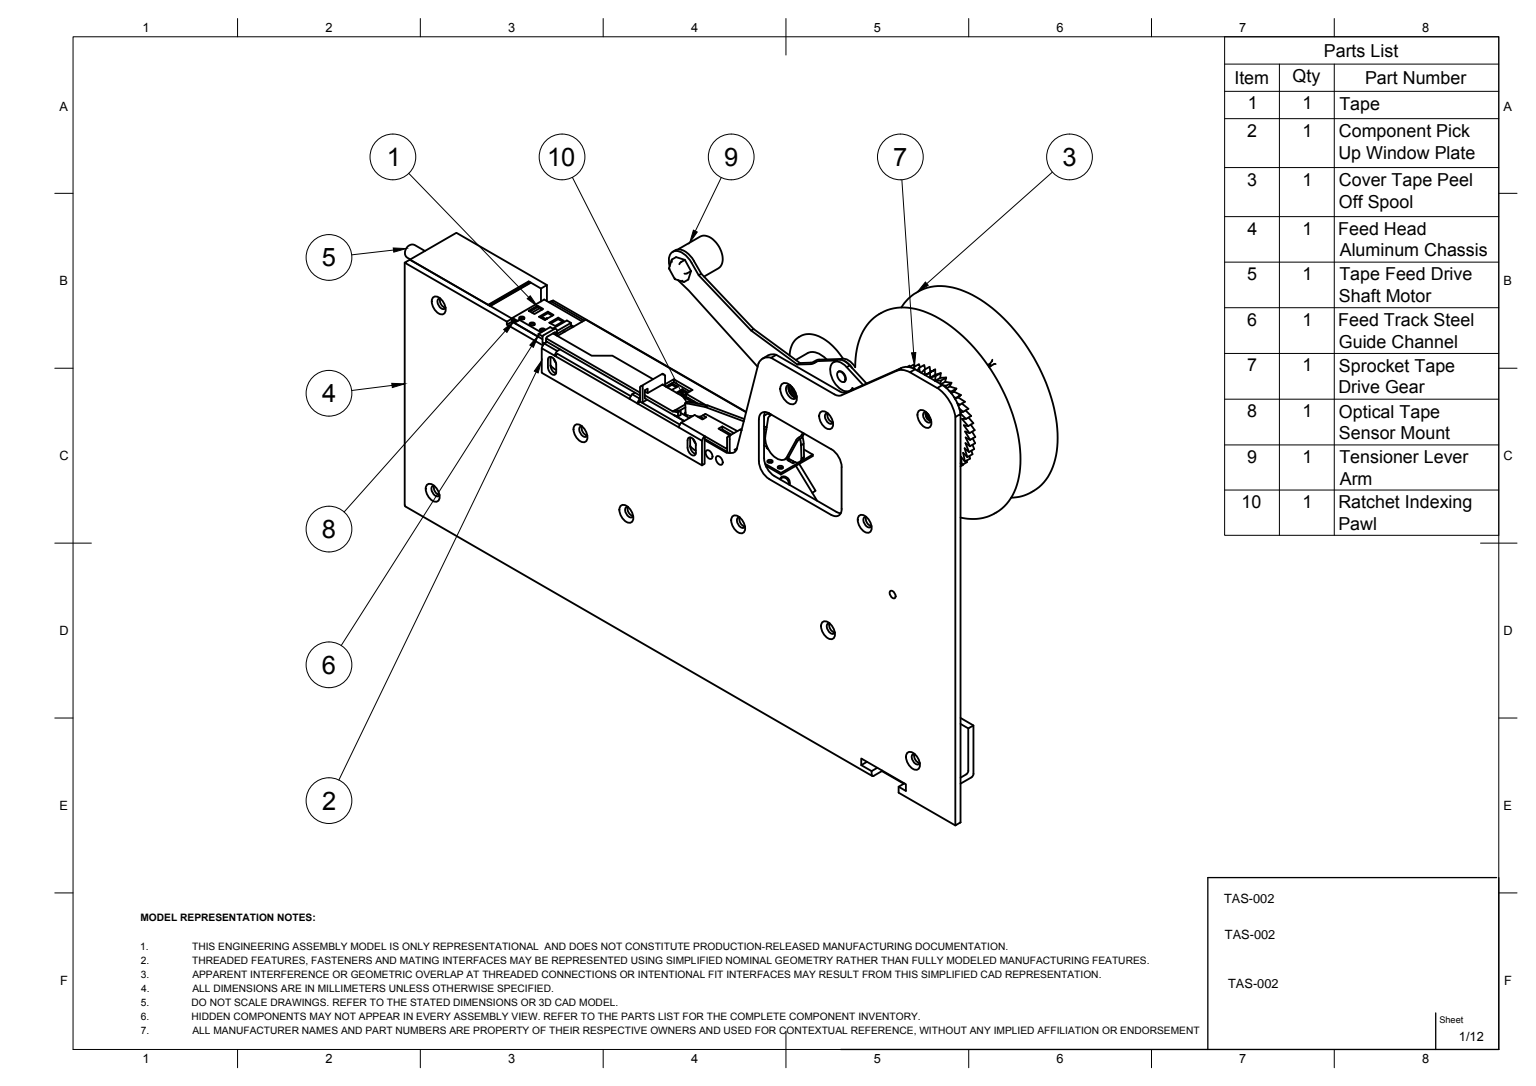
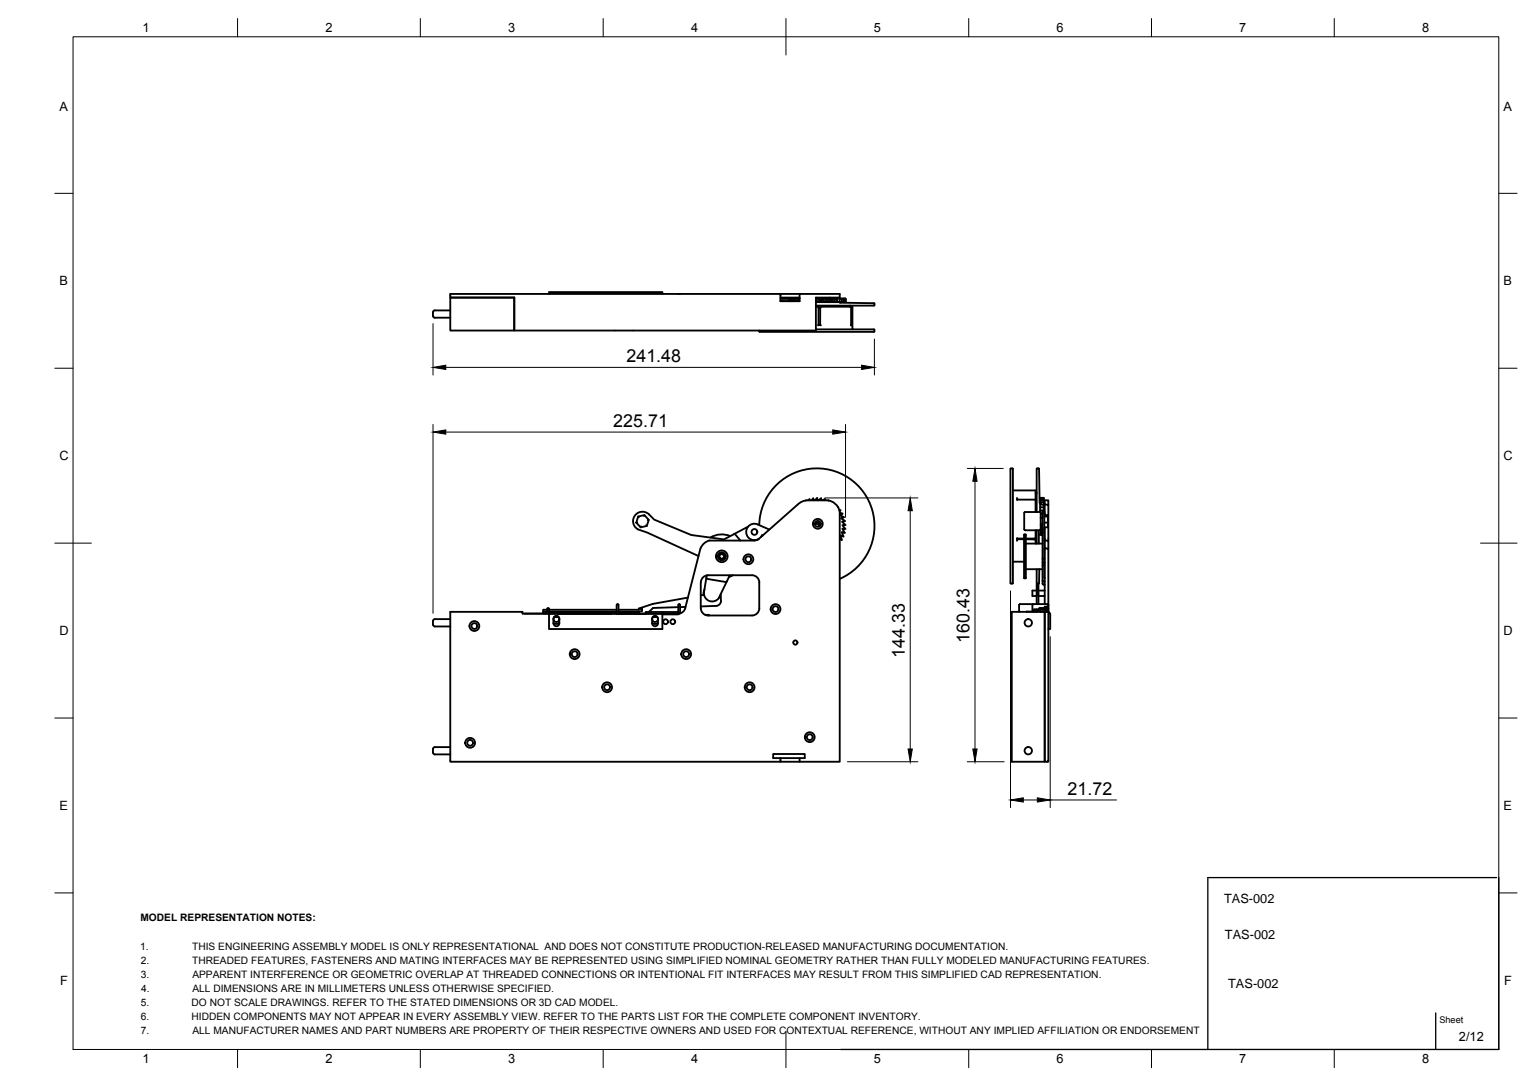
ISO-10303-21;
HEADER;
/* Generated by software containing ST-Developer
 * from STEP Tools, Inc. (www.steptools.com) 
 */

FILE_DESCRIPTION(
/* description */ ('STEP AP214'),
/* implementation_level */ '2;1');

FILE_NAME(
/* name */ 'TAS-002',
/* time_stamp */ '2026-11-04T19:38:14-08:00',
/* author */ (''),
/* organization */ (''),
/* preprocessor_version */ 'ST-DEVELOPER v20.2',
/* originating_system */ 'Autodesk Translation Framework v15.17.0.0',
/* authorisation */ '');

FILE_SCHEMA (('AUTOMOTIVE_DESIGN { 1 0 10303 214 3 1 1 }'));
ENDSEC;

DATA;
#10=MECHANICAL_DESIGN_GEOMETRIC_PRESENTATION_REPRESENTATION('',(#470,#471,
#472,#473,#474,#475,#476,#477,#478,#479),#36668);
#11=ITEM_DEFINED_TRANSFORMATION($,$,#17916,#19428);
#12=ITEM_DEFINED_TRANSFORMATION($,$,#18105,#19429);
#13=ITEM_DEFINED_TRANSFORMATION($,$,#18270,#19430);
#14=ITEM_DEFINED_TRANSFORMATION($,$,#18564,#19431);
#15=ITEM_DEFINED_TRANSFORMATION($,$,#18726,#19432);
#16=ITEM_DEFINED_TRANSFORMATION($,$,#18755,#19433);
#17=ITEM_DEFINED_TRANSFORMATION($,$,#18787,#19434);
#18=ITEM_DEFINED_TRANSFORMATION($,$,#19085,#19435);
#19=ITEM_DEFINED_TRANSFORMATION($,$,#19168,#19436);
#20=ITEM_DEFINED_TRANSFORMATION($,$,#19405,#19437);
#21=(
REPRESENTATION_RELATIONSHIP($,$,#36706,#36705)
REPRESENTATION_RELATIONSHIP_WITH_TRANSFORMATION(#11)
SHAPE_REPRESENTATION_RELATIONSHIP()
);
#22=(
REPRESENTATION_RELATIONSHIP($,$,#36707,#36705)
REPRESENTATION_RELATIONSHIP_WITH_TRANSFORMATION(#12)
SHAPE_REPRESENTATION_RELATIONSHIP()
);
#23=(
REPRESENTATION_RELATIONSHIP($,$,#36708,#36705)
REPRESENTATION_RELATIONSHIP_WITH_TRANSFORMATION(#13)
SHAPE_REPRESENTATION_RELATIONSHIP()
);
#24=(
REPRESENTATION_RELATIONSHIP($,$,#36709,#36705)
REPRESENTATION_RELATIONSHIP_WITH_TRANSFORMATION(#14)
SHAPE_REPRESENTATION_RELATIONSHIP()
);
#25=(
REPRESENTATION_RELATIONSHIP($,$,#36710,#36705)
REPRESENTATION_RELATIONSHIP_WITH_TRANSFORMATION(#15)
SHAPE_REPRESENTATION_RELATIONSHIP()
);
#26=(
REPRESENTATION_RELATIONSHIP($,$,#36711,#36705)
REPRESENTATION_RELATIONSHIP_WITH_TRANSFORMATION(#16)
SHAPE_REPRESENTATION_RELATIONSHIP()
);
#27=(
REPRESENTATION_RELATIONSHIP($,$,#36712,#36705)
REPRESENTATION_RELATIONSHIP_WITH_TRANSFORMATION(#17)
SHAPE_REPRESENTATION_RELATIONSHIP()
);
#28=(
REPRESENTATION_RELATIONSHIP($,$,#36713,#36705)
REPRESENTATION_RELATIONSHIP_WITH_TRANSFORMATION(#18)
SHAPE_REPRESENTATION_RELATIONSHIP()
);
#29=(
REPRESENTATION_RELATIONSHIP($,$,#36714,#36705)
REPRESENTATION_RELATIONSHIP_WITH_TRANSFORMATION(#19)
SHAPE_REPRESENTATION_RELATIONSHIP()
);
#30=(
REPRESENTATION_RELATIONSHIP($,$,#36715,#36705)
REPRESENTATION_RELATIONSHIP_WITH_TRANSFORMATION(#20)
SHAPE_REPRESENTATION_RELATIONSHIP()
);
#31=CONTEXT_DEPENDENT_SHAPE_REPRESENTATION(#21,#36695);
#32=CONTEXT_DEPENDENT_SHAPE_REPRESENTATION(#22,#36696);
#33=CONTEXT_DEPENDENT_SHAPE_REPRESENTATION(#23,#36697);
#34=CONTEXT_DEPENDENT_SHAPE_REPRESENTATION(#24,#36698);
#35=CONTEXT_DEPENDENT_SHAPE_REPRESENTATION(#25,#36699);
#36=CONTEXT_DEPENDENT_SHAPE_REPRESENTATION(#26,#36700);
#37=CONTEXT_DEPENDENT_SHAPE_REPRESENTATION(#27,#36701);
#38=CONTEXT_DEPENDENT_SHAPE_REPRESENTATION(#28,#36702);
#39=CONTEXT_DEPENDENT_SHAPE_REPRESENTATION(#29,#36703);
#40=CONTEXT_DEPENDENT_SHAPE_REPRESENTATION(#30,#36704);
#41=NEXT_ASSEMBLY_USAGE_OCCURRENCE('Tape:1','Tape:1','Tape:1',#36717,#36718,
'Tape:1');
#42=NEXT_ASSEMBLY_USAGE_OCCURRENCE('Component Pick Up Window Plate:1',
'Component Pick Up Window Plate:1','Component Pick Up Window Plate:1',#36717,
#36719,'Component Pick Up Window Plate:1');
#43=NEXT_ASSEMBLY_USAGE_OCCURRENCE('Cover Tape Peel Off Spool:1',
'Cover Tape Peel Off Spool:1','Cover Tape Peel Off Spool:1',#36717,#36720,
'Cover Tape Peel Off Spool:1');
#44=NEXT_ASSEMBLY_USAGE_OCCURRENCE('Feed Head Aluminum Chassis:1',
'Feed Head Aluminum Chassis:1','Feed Head Aluminum Chassis:1',#36717,#36721,
'Feed Head Aluminum Chassis:1');
#45=NEXT_ASSEMBLY_USAGE_OCCURRENCE('Tape Feed Drive Shaft Motor:1',
'Tape Feed Drive Shaft Motor:1','Tape Feed Drive Shaft Motor:1',#36717,
#36722,'Tape Feed Drive Shaft Motor:1');
#46=NEXT_ASSEMBLY_USAGE_OCCURRENCE('Feed Track Steel Guide Channel:1',
'Feed Track Steel Guide Channel:1','Feed Track Steel Guide Channel:1',#36717,
#36723,'Feed Track Steel Guide Channel:1');
#47=NEXT_ASSEMBLY_USAGE_OCCURRENCE('Sprocket Tape Drive Gear:1',
'Sprocket Tape Drive Gear:1','Sprocket Tape Drive Gear:1',#36717,#36724,
'Sprocket Tape Drive Gear:1');
#48=NEXT_ASSEMBLY_USAGE_OCCURRENCE('Optical Tape Sensor Mount:1',
'Optical Tape Sensor Mount:1','Optical Tape Sensor Mount:1',#36717,#36725,
'Optical Tape Sensor Mount:1');
#49=NEXT_ASSEMBLY_USAGE_OCCURRENCE('Tensioner Lever Arm:1',
'Tensioner Lever Arm:1','Tensioner Lever Arm:1',#36717,#36726,
'Tensioner Lever Arm:1');
#50=NEXT_ASSEMBLY_USAGE_OCCURRENCE('Ratchet Indexing Pawl:1',
'Ratchet Indexing Pawl:1','Ratchet Indexing Pawl:1',#36717,#36727,
'Ratchet Indexing Pawl:1');
#51=ORIENTED_CLOSED_SHELL('',*,#17801,.F.);
#52=BREP_WITH_VOIDS('Body1',#17802,(#51));
#53=B_SPLINE_SURFACE_WITH_KNOTS('',3,1,((#33152,#33153),(#33154,#33155),
(#33156,#33157),(#33158,#33159),(#33160,#33161),(#33162,#33163),(#33164,
#33165),(#33166,#33167),(#33168,#33169),(#33170,#33171),(#33172,#33173),
(#33174,#33175),(#33176,#33177),(#33178,#33179),(#33180,#33181),(#33182,
#33183),(#33184,#33185),(#33186,#33187),(#33188,#33189)),.UNSPECIFIED.,
 .F.,.F.,.F.,(4,1,1,1,1,1,1,1,1,1,1,1,1,1,1,1,4),(2,2),(0.,0.0619654006870562,
0.122121905638296,0.180988496849837,0.239933216451894,0.299905831106524,
0.359988847476984,0.421775741741642,0.486575826421121,0.551534804619736,
0.615017542759975,0.677258616661654,0.739729962362713,0.803050102662949,
0.866495132015699,0.931973474177149,1.),(0.,0.0239999999999995),
 .UNSPECIFIED.);
#54=B_SPLINE_SURFACE_WITH_KNOTS('',3,1,((#33213,#33214),(#33215,#33216),
(#33217,#33218),(#33219,#33220),(#33221,#33222),(#33223,#33224),(#33225,
#33226),(#33227,#33228),(#33229,#33230),(#33231,#33232),(#33233,#33234),
(#33235,#33236),(#33237,#33238),(#33239,#33240),(#33241,#33242)),
 .UNSPECIFIED.,.F.,.F.,.F.,(4,1,1,1,1,1,1,1,1,1,1,1,4),(2,2),(0.,0.110802643801324,
0.212829202347773,0.306101309823115,0.390647321116006,0.46692446936085,
0.534481039284033,0.593586940965671,0.644557004508714,0.736200452629367,
0.825024025618864,0.911985584829753,1.),(0.,0.0239999999999995),
 .UNSPECIFIED.);
#55=B_SPLINE_SURFACE_WITH_KNOTS('',3,1,((#33280,#33281),(#33282,#33283),
(#33284,#33285),(#33286,#33287),(#33288,#33289),(#33290,#33291),(#33292,
#33293),(#33294,#33295),(#33296,#33297),(#33298,#33299),(#33300,#33301),
(#33302,#33303),(#33304,#33305),(#33306,#33307),(#33308,#33309)),
 .UNSPECIFIED.,.F.,.F.,.F.,(4,1,1,1,1,1,1,1,1,1,1,1,4),(2,2),(0.,0.0987013748863702,
0.195670680385855,0.292419992908961,0.391339286967469,0.444458741764931,
0.504224579154748,0.570347591406357,0.642913825979479,0.722289816523959,
0.807922721202247,0.900470366297794,1.),(0.,0.0239999999999995),
 .UNSPECIFIED.);
#56=B_SPLINE_SURFACE_WITH_KNOTS('',3,1,((#33327,#33328),(#33329,#33330),
(#33331,#33332),(#33333,#33334),(#33335,#33336),(#33337,#33338),(#33339,
#33340),(#33341,#33342),(#33343,#33344),(#33345,#33346),(#33347,#33348),
(#33349,#33350),(#33351,#33352),(#33353,#33354),(#33355,#33356),(#33357,
#33358),(#33359,#33360),(#33361,#33362),(#33363,#33364)),.UNSPECIFIED.,
 .F.,.F.,.F.,(4,1,1,1,1,1,1,1,1,1,1,1,1,1,1,1,4),(2,2),(0.,0.0694796363669832,
0.136525003539142,0.200800892873422,0.263983206913328,0.325711144761188,
0.38727051407573,0.449492780531563,0.51295519576285,0.576266397070109,0.637574966831173,
0.697901098424494,0.757558279411561,0.81658750436506,0.876645756608308,
0.937285872938128,1.),(0.,0.0240000000000054),.UNSPECIFIED.);
#57=B_SPLINE_SURFACE_WITH_KNOTS('',3,1,((#33386,#33387),(#33388,#33389),
(#33390,#33391),(#33392,#33393),(#33394,#33395),(#33396,#33397),(#33398,
#33399),(#33400,#33401),(#33402,#33403),(#33404,#33405),(#33406,#33407),
(#33408,#33409),(#33410,#33411),(#33412,#33413),(#33414,#33415),(#33416,
#33417),(#33418,#33419),(#33420,#33421),(#33422,#33423)),.UNSPECIFIED.,
 .F.,.F.,.F.,(4,1,1,1,1,1,1,1,1,1,1,1,1,1,1,1,4),(2,2),(0.,0.0687907943906199,
0.135103289431132,0.198978674310652,0.261904299780862,0.323494969367974,
0.385195377966055,0.446969238740777,0.509764776703136,0.572250568847369,
0.633405175661155,0.693251162921754,0.752583162785671,0.812579266153423,
0.873275084920192,0.93554994289503,1.),(0.,0.0239999999999995),
 .UNSPECIFIED.);
#58=B_SPLINE_SURFACE_WITH_KNOTS('',3,1,((#33449,#33450),(#33451,#33452),
(#33453,#33454),(#33455,#33456),(#33457,#33458),(#33459,#33460),(#33461,
#33462),(#33463,#33464),(#33465,#33466),(#33467,#33468),(#33469,#33470),
(#33471,#33472),(#33473,#33474),(#33475,#33476),(#33477,#33478),(#33479,
#33480),(#33481,#33482),(#33483,#33484),(#33485,#33486)),.UNSPECIFIED.,
 .F.,.F.,.F.,(4,1,1,1,1,1,1,1,1,1,1,1,1,1,1,1,4),(2,2),(0.,0.064429890715421,
0.126529667073554,0.186743666835525,0.245897683478137,0.304053106820992,
0.362195516217047,0.420654638852463,0.480330856318868,0.540662876085596,
0.600743511343268,0.661981856833518,0.724480055372708,0.789067141037209,
0.856333336778513,0.926362064011592,1.),(0.,0.0239999999999995),
 .UNSPECIFIED.);
#59=(
BOUNDED_CURVE()
B_SPLINE_CURVE(2,(#28963,#28964,#28965,#28966,#28967,#28968,#28969),
 .UNSPECIFIED.,.F.,.F.)
B_SPLINE_CURVE_WITH_KNOTS((3,2,2,3),(0.975,0.983333333333333,0.991666666666667,
1.),.UNSPECIFIED.)
CURVE()
GEOMETRIC_REPRESENTATION_ITEM()
RATIONAL_B_SPLINE_CURVE((1.,0.866025403784439,1.,0.866025403784439,1.,0.866025403784439,
1.))
REPRESENTATION_ITEM('')
);
#60=(
BOUNDED_CURVE()
B_SPLINE_CURVE(2,(#28975,#28976,#28977,#28978,#28979,#28980,#28981),
 .UNSPECIFIED.,.F.,.F.)
B_SPLINE_CURVE_WITH_KNOTS((3,2,2,3),(0.975,0.983333333333333,0.991666666666667,
1.),.UNSPECIFIED.)
CURVE()
GEOMETRIC_REPRESENTATION_ITEM()
RATIONAL_B_SPLINE_CURVE((1.,0.866025403784439,1.,0.866025403784439,1.,0.866025403784439,
1.))
REPRESENTATION_ITEM('')
);
#61=(
BOUNDED_CURVE()
B_SPLINE_CURVE(2,(#28984,#28985,#28986,#28987,#28988,#28989,#28990),
 .UNSPECIFIED.,.F.,.F.)
B_SPLINE_CURVE_WITH_KNOTS((3,2,2,3),(0.975,0.983333333333333,0.991666666666667,
1.),.UNSPECIFIED.)
CURVE()
GEOMETRIC_REPRESENTATION_ITEM()
RATIONAL_B_SPLINE_CURVE((1.,0.866025403784439,1.,0.866025403784439,1.,0.866025403784439,
1.))
REPRESENTATION_ITEM('')
);
#62=(
BOUNDED_CURVE()
B_SPLINE_CURVE(2,(#28995,#28996,#28997,#28998,#28999,#29000,#29001,#29002,
#29003,#29004,#29005,#29006,#29007),.UNSPECIFIED.,.F.,.F.)
B_SPLINE_CURVE_WITH_KNOTS((3,2,2,2,2,2,3),(0.925,0.933333333333333,0.941666666666667,
0.95,0.958333333333333,0.966666666666667,0.975),.UNSPECIFIED.)
CURVE()
GEOMETRIC_REPRESENTATION_ITEM()
RATIONAL_B_SPLINE_CURVE((1.,0.866025403784439,1.,0.866025403784439,1.,0.866025403784439,
1.,0.866025403784439,1.,0.866025403784439,1.,0.866025403784439,1.))
REPRESENTATION_ITEM('')
);
#63=(
BOUNDED_CURVE()
B_SPLINE_CURVE(2,(#29008,#29009,#29010,#29011,#29012,#29013,#29014,#29015,
#29016,#29017,#29018,#29019,#29020),.UNSPECIFIED.,.F.,.F.)
B_SPLINE_CURVE_WITH_KNOTS((3,2,2,2,2,2,3),(0.925,0.933333333333333,0.941666666666667,
0.95,0.958333333333333,0.966666666666667,0.975),.UNSPECIFIED.)
CURVE()
GEOMETRIC_REPRESENTATION_ITEM()
RATIONAL_B_SPLINE_CURVE((1.,0.866025403784439,1.,0.866025403784439,1.,0.866025403784439,
1.,0.866025403784439,1.,0.866025403784439,1.,0.866025403784439,1.))
REPRESENTATION_ITEM('')
);
#64=(
BOUNDED_CURVE()
B_SPLINE_CURVE(2,(#29025,#29026,#29027,#29028,#29029,#29030,#29031,#29032,
#29033,#29034,#29035,#29036,#29037),.UNSPECIFIED.,.F.,.F.)
B_SPLINE_CURVE_WITH_KNOTS((3,2,2,2,2,2,3),(0.875,0.883333333333333,0.891666666666667,
0.9,0.908333333333333,0.916666666666667,0.925),.UNSPECIFIED.)
CURVE()
GEOMETRIC_REPRESENTATION_ITEM()
RATIONAL_B_SPLINE_CURVE((1.,0.866025403784439,1.,0.866025403784439,1.,0.866025403784439,
1.,0.866025403784439,1.,0.866025403784439,1.,0.866025403784439,1.))
REPRESENTATION_ITEM('')
);
#65=(
BOUNDED_CURVE()
B_SPLINE_CURVE(2,(#29038,#29039,#29040,#29041,#29042,#29043,#29044,#29045,
#29046,#29047,#29048,#29049,#29050),.UNSPECIFIED.,.F.,.F.)
B_SPLINE_CURVE_WITH_KNOTS((3,2,2,2,2,2,3),(0.875,0.883333333333333,0.891666666666667,
0.9,0.908333333333333,0.916666666666667,0.925),.UNSPECIFIED.)
CURVE()
GEOMETRIC_REPRESENTATION_ITEM()
RATIONAL_B_SPLINE_CURVE((1.,0.866025403784439,1.,0.866025403784439,1.,0.866025403784439,
1.,0.866025403784439,1.,0.866025403784439,1.,0.866025403784439,1.))
REPRESENTATION_ITEM('')
);
#66=(
BOUNDED_CURVE()
B_SPLINE_CURVE(2,(#29055,#29056,#29057,#29058,#29059,#29060,#29061,#29062,
#29063,#29064,#29065,#29066,#29067),.UNSPECIFIED.,.F.,.F.)
B_SPLINE_CURVE_WITH_KNOTS((3,2,2,2,2,2,3),(0.825,0.833333333333333,0.841666666666667,
0.85,0.858333333333333,0.866666666666667,0.875),.UNSPECIFIED.)
CURVE()
GEOMETRIC_REPRESENTATION_ITEM()
RATIONAL_B_SPLINE_CURVE((1.,0.866025403784439,1.,0.866025403784439,1.,0.866025403784439,
1.,0.866025403784439,1.,0.866025403784439,1.,0.866025403784439,1.))
REPRESENTATION_ITEM('')
);
#67=(
BOUNDED_CURVE()
B_SPLINE_CURVE(2,(#29068,#29069,#29070,#29071,#29072,#29073,#29074,#29075,
#29076,#29077,#29078,#29079,#29080),.UNSPECIFIED.,.F.,.F.)
B_SPLINE_CURVE_WITH_KNOTS((3,2,2,2,2,2,3),(0.825,0.833333333333333,0.841666666666667,
0.85,0.858333333333333,0.866666666666667,0.875),.UNSPECIFIED.)
CURVE()
GEOMETRIC_REPRESENTATION_ITEM()
RATIONAL_B_SPLINE_CURVE((1.,0.866025403784439,1.,0.866025403784439,1.,0.866025403784439,
1.,0.866025403784439,1.,0.866025403784439,1.,0.866025403784439,1.))
REPRESENTATION_ITEM('')
);
#68=(
BOUNDED_CURVE()
B_SPLINE_CURVE(2,(#29085,#29086,#29087,#29088,#29089,#29090,#29091,#29092,
#29093,#29094,#29095,#29096,#29097),.UNSPECIFIED.,.F.,.F.)
B_SPLINE_CURVE_WITH_KNOTS((3,2,2,2,2,2,3),(0.775,0.783333333333333,0.791666666666667,
0.8,0.808333333333333,0.816666666666667,0.825),.UNSPECIFIED.)
CURVE()
GEOMETRIC_REPRESENTATION_ITEM()
RATIONAL_B_SPLINE_CURVE((1.,0.866025403784439,1.,0.866025403784439,1.,0.866025403784439,
1.,0.866025403784439,1.,0.866025403784439,1.,0.866025403784439,1.))
REPRESENTATION_ITEM('')
);
#69=(
BOUNDED_CURVE()
B_SPLINE_CURVE(2,(#29098,#29099,#29100,#29101,#29102,#29103,#29104,#29105,
#29106,#29107,#29108,#29109,#29110),.UNSPECIFIED.,.F.,.F.)
B_SPLINE_CURVE_WITH_KNOTS((3,2,2,2,2,2,3),(0.775,0.783333333333333,0.791666666666667,
0.8,0.808333333333333,0.816666666666667,0.825),.UNSPECIFIED.)
CURVE()
GEOMETRIC_REPRESENTATION_ITEM()
RATIONAL_B_SPLINE_CURVE((1.,0.866025403784439,1.,0.866025403784439,1.,0.866025403784439,
1.,0.866025403784439,1.,0.866025403784439,1.,0.866025403784439,1.))
REPRESENTATION_ITEM('')
);
#70=(
BOUNDED_CURVE()
B_SPLINE_CURVE(2,(#29115,#29116,#29117,#29118,#29119,#29120,#29121,#29122,
#29123,#29124,#29125,#29126,#29127),.UNSPECIFIED.,.F.,.F.)
B_SPLINE_CURVE_WITH_KNOTS((3,2,2,2,2,2,3),(0.725,0.733333333333333,0.741666666666667,
0.75,0.758333333333333,0.766666666666667,0.775),.UNSPECIFIED.)
CURVE()
GEOMETRIC_REPRESENTATION_ITEM()
RATIONAL_B_SPLINE_CURVE((1.,0.866025403784439,1.,0.866025403784439,1.,0.866025403784439,
1.,0.866025403784439,1.,0.866025403784439,1.,0.866025403784439,1.))
REPRESENTATION_ITEM('')
);
#71=(
BOUNDED_CURVE()
B_SPLINE_CURVE(2,(#29128,#29129,#29130,#29131,#29132,#29133,#29134,#29135,
#29136,#29137,#29138,#29139,#29140),.UNSPECIFIED.,.F.,.F.)
B_SPLINE_CURVE_WITH_KNOTS((3,2,2,2,2,2,3),(0.725,0.733333333333333,0.741666666666667,
0.75,0.758333333333333,0.766666666666667,0.775),.UNSPECIFIED.)
CURVE()
GEOMETRIC_REPRESENTATION_ITEM()
RATIONAL_B_SPLINE_CURVE((1.,0.866025403784439,1.,0.866025403784439,1.,0.866025403784439,
1.,0.866025403784439,1.,0.866025403784439,1.,0.866025403784439,1.))
REPRESENTATION_ITEM('')
);
#72=(
BOUNDED_CURVE()
B_SPLINE_CURVE(2,(#29145,#29146,#29147,#29148,#29149,#29150,#29151,#29152,
#29153,#29154,#29155,#29156,#29157),.UNSPECIFIED.,.F.,.F.)
B_SPLINE_CURVE_WITH_KNOTS((3,2,2,2,2,2,3),(0.675,0.683333333333333,0.691666666666667,
0.7,0.708333333333333,0.716666666666667,0.725),.UNSPECIFIED.)
CURVE()
GEOMETRIC_REPRESENTATION_ITEM()
RATIONAL_B_SPLINE_CURVE((1.,0.866025403784439,1.,0.866025403784439,1.,0.866025403784439,
1.,0.866025403784439,1.,0.866025403784439,1.,0.866025403784439,1.))
REPRESENTATION_ITEM('')
);
#73=(
BOUNDED_CURVE()
B_SPLINE_CURVE(2,(#29158,#29159,#29160,#29161,#29162,#29163,#29164,#29165,
#29166,#29167,#29168,#29169,#29170),.UNSPECIFIED.,.F.,.F.)
B_SPLINE_CURVE_WITH_KNOTS((3,2,2,2,2,2,3),(0.675,0.683333333333333,0.691666666666667,
0.7,0.708333333333333,0.716666666666667,0.725),.UNSPECIFIED.)
CURVE()
GEOMETRIC_REPRESENTATION_ITEM()
RATIONAL_B_SPLINE_CURVE((1.,0.866025403784439,1.,0.866025403784439,1.,0.866025403784439,
1.,0.866025403784439,1.,0.866025403784439,1.,0.866025403784439,1.))
REPRESENTATION_ITEM('')
);
#74=(
BOUNDED_CURVE()
B_SPLINE_CURVE(2,(#29175,#29176,#29177,#29178,#29179,#29180,#29181,#29182,
#29183,#29184,#29185,#29186,#29187),.UNSPECIFIED.,.F.,.F.)
B_SPLINE_CURVE_WITH_KNOTS((3,2,2,2,2,2,3),(0.625,0.633333333333333,0.641666666666667,
0.65,0.658333333333333,0.666666666666667,0.675),.UNSPECIFIED.)
CURVE()
GEOMETRIC_REPRESENTATION_ITEM()
RATIONAL_B_SPLINE_CURVE((1.,0.866025403784439,1.,0.866025403784439,1.,0.866025403784439,
1.,0.866025403784439,1.,0.866025403784439,1.,0.866025403784439,1.))
REPRESENTATION_ITEM('')
);
#75=(
BOUNDED_CURVE()
B_SPLINE_CURVE(2,(#29188,#29189,#29190,#29191,#29192,#29193,#29194,#29195,
#29196,#29197,#29198,#29199,#29200),.UNSPECIFIED.,.F.,.F.)
B_SPLINE_CURVE_WITH_KNOTS((3,2,2,2,2,2,3),(0.625,0.633333333333333,0.641666666666667,
0.65,0.658333333333333,0.666666666666667,0.675),.UNSPECIFIED.)
CURVE()
GEOMETRIC_REPRESENTATION_ITEM()
RATIONAL_B_SPLINE_CURVE((1.,0.866025403784439,1.,0.866025403784439,1.,0.866025403784439,
1.,0.866025403784439,1.,0.866025403784439,1.,0.866025403784439,1.))
REPRESENTATION_ITEM('')
);
#76=(
BOUNDED_CURVE()
B_SPLINE_CURVE(2,(#29205,#29206,#29207,#29208,#29209,#29210,#29211,#29212,
#29213,#29214,#29215,#29216,#29217),.UNSPECIFIED.,.F.,.F.)
B_SPLINE_CURVE_WITH_KNOTS((3,2,2,2,2,2,3),(0.575,0.583333333333333,0.591666666666667,
0.6,0.608333333333333,0.616666666666667,0.625),.UNSPECIFIED.)
CURVE()
GEOMETRIC_REPRESENTATION_ITEM()
RATIONAL_B_SPLINE_CURVE((1.,0.866025403784439,1.,0.866025403784439,1.,0.866025403784439,
1.,0.866025403784439,1.,0.866025403784439,1.,0.866025403784439,1.))
REPRESENTATION_ITEM('')
);
#77=(
BOUNDED_CURVE()
B_SPLINE_CURVE(2,(#29218,#29219,#29220,#29221,#29222,#29223,#29224,#29225,
#29226,#29227,#29228,#29229,#29230),.UNSPECIFIED.,.F.,.F.)
B_SPLINE_CURVE_WITH_KNOTS((3,2,2,2,2,2,3),(0.575,0.583333333333333,0.591666666666667,
0.6,0.608333333333333,0.616666666666667,0.625),.UNSPECIFIED.)
CURVE()
GEOMETRIC_REPRESENTATION_ITEM()
RATIONAL_B_SPLINE_CURVE((1.,0.866025403784439,1.,0.866025403784439,1.,0.866025403784439,
1.,0.866025403784439,1.,0.866025403784439,1.,0.866025403784439,1.))
REPRESENTATION_ITEM('')
);
#78=(
BOUNDED_CURVE()
B_SPLINE_CURVE(2,(#29235,#29236,#29237,#29238,#29239,#29240,#29241,#29242,
#29243,#29244,#29245,#29246,#29247),.UNSPECIFIED.,.F.,.F.)
B_SPLINE_CURVE_WITH_KNOTS((3,2,2,2,2,2,3),(0.525,0.533333333333333,0.541666666666667,
0.55,0.558333333333333,0.566666666666667,0.575),.UNSPECIFIED.)
CURVE()
GEOMETRIC_REPRESENTATION_ITEM()
RATIONAL_B_SPLINE_CURVE((1.,0.866025403784439,1.,0.866025403784439,1.,0.866025403784439,
1.,0.866025403784439,1.,0.866025403784439,1.,0.866025403784439,1.))
REPRESENTATION_ITEM('')
);
#79=(
BOUNDED_CURVE()
B_SPLINE_CURVE(2,(#29248,#29249,#29250,#29251,#29252,#29253,#29254,#29255,
#29256,#29257,#29258,#29259,#29260),.UNSPECIFIED.,.F.,.F.)
B_SPLINE_CURVE_WITH_KNOTS((3,2,2,2,2,2,3),(0.525,0.533333333333333,0.541666666666667,
0.55,0.558333333333333,0.566666666666667,0.575),.UNSPECIFIED.)
CURVE()
GEOMETRIC_REPRESENTATION_ITEM()
RATIONAL_B_SPLINE_CURVE((1.,0.866025403784439,1.,0.866025403784439,1.,0.866025403784439,
1.,0.866025403784439,1.,0.866025403784439,1.,0.866025403784439,1.))
REPRESENTATION_ITEM('')
);
#80=(
BOUNDED_CURVE()
B_SPLINE_CURVE(2,(#29265,#29266,#29267,#29268,#29269,#29270,#29271,#29272,
#29273,#29274,#29275,#29276,#29277),.UNSPECIFIED.,.F.,.F.)
B_SPLINE_CURVE_WITH_KNOTS((3,2,2,2,2,2,3),(0.475,0.483333333333333,0.491666666666667,
0.5,0.508333333333333,0.516666666666667,0.525),.UNSPECIFIED.)
CURVE()
GEOMETRIC_REPRESENTATION_ITEM()
RATIONAL_B_SPLINE_CURVE((1.,0.866025403784439,1.,0.866025403784439,1.,0.866025403784439,
1.,0.866025403784439,1.,0.866025403784439,1.,0.866025403784439,1.))
REPRESENTATION_ITEM('')
);
#81=(
BOUNDED_CURVE()
B_SPLINE_CURVE(2,(#29278,#29279,#29280,#29281,#29282,#29283,#29284,#29285,
#29286,#29287,#29288,#29289,#29290),.UNSPECIFIED.,.F.,.F.)
B_SPLINE_CURVE_WITH_KNOTS((3,2,2,2,2,2,3),(0.475,0.483333333333333,0.491666666666667,
0.5,0.508333333333333,0.516666666666667,0.525),.UNSPECIFIED.)
CURVE()
GEOMETRIC_REPRESENTATION_ITEM()
RATIONAL_B_SPLINE_CURVE((1.,0.866025403784439,1.,0.866025403784439,1.,0.866025403784439,
1.,0.866025403784439,1.,0.866025403784439,1.,0.866025403784439,1.))
REPRESENTATION_ITEM('')
);
#82=(
BOUNDED_CURVE()
B_SPLINE_CURVE(2,(#29295,#29296,#29297,#29298,#29299,#29300,#29301,#29302,
#29303,#29304,#29305,#29306,#29307),.UNSPECIFIED.,.F.,.F.)
B_SPLINE_CURVE_WITH_KNOTS((3,2,2,2,2,2,3),(0.425,0.433333333333334,0.441666666666666,
0.45,0.458333333333333,0.466666666666667,0.475),.UNSPECIFIED.)
CURVE()
GEOMETRIC_REPRESENTATION_ITEM()
RATIONAL_B_SPLINE_CURVE((1.,0.866025403784439,1.,0.866025403784439,1.,0.866025403784439,
1.,0.866025403784439,1.,0.866025403784439,1.,0.866025403784439,1.))
REPRESENTATION_ITEM('')
);
#83=(
BOUNDED_CURVE()
B_SPLINE_CURVE(2,(#29308,#29309,#29310,#29311,#29312,#29313,#29314,#29315,
#29316,#29317,#29318,#29319,#29320),.UNSPECIFIED.,.F.,.F.)
B_SPLINE_CURVE_WITH_KNOTS((3,2,2,2,2,2,3),(0.425,0.433333333333334,0.441666666666666,
0.45,0.458333333333333,0.466666666666667,0.475),.UNSPECIFIED.)
CURVE()
GEOMETRIC_REPRESENTATION_ITEM()
RATIONAL_B_SPLINE_CURVE((1.,0.866025403784439,1.,0.866025403784439,1.,0.866025403784439,
1.,0.866025403784439,1.,0.866025403784439,1.,0.866025403784439,1.))
REPRESENTATION_ITEM('')
);
#84=(
BOUNDED_CURVE()
B_SPLINE_CURVE(2,(#29325,#29326,#29327,#29328,#29329,#29330,#29331,#29332,
#29333,#29334,#29335,#29336,#29337),.UNSPECIFIED.,.F.,.F.)
B_SPLINE_CURVE_WITH_KNOTS((3,2,2,2,2,2,3),(0.375,0.383333333333334,0.391666666666666,
0.4,0.408333333333334,0.416666666666667,0.425),.UNSPECIFIED.)
CURVE()
GEOMETRIC_REPRESENTATION_ITEM()
RATIONAL_B_SPLINE_CURVE((1.,0.866025403784439,1.,0.866025403784439,1.,0.866025403784439,
1.,0.866025403784439,1.,0.866025403784439,1.,0.866025403784439,1.))
REPRESENTATION_ITEM('')
);
#85=(
BOUNDED_CURVE()
B_SPLINE_CURVE(2,(#29338,#29339,#29340,#29341,#29342,#29343,#29344,#29345,
#29346,#29347,#29348,#29349,#29350),.UNSPECIFIED.,.F.,.F.)
B_SPLINE_CURVE_WITH_KNOTS((3,2,2,2,2,2,3),(0.375,0.383333333333334,0.391666666666666,
0.4,0.408333333333334,0.416666666666667,0.425),.UNSPECIFIED.)
CURVE()
GEOMETRIC_REPRESENTATION_ITEM()
RATIONAL_B_SPLINE_CURVE((1.,0.866025403784439,1.,0.866025403784439,1.,0.866025403784439,
1.,0.866025403784439,1.,0.866025403784439,1.,0.866025403784439,1.))
REPRESENTATION_ITEM('')
);
#86=(
BOUNDED_CURVE()
B_SPLINE_CURVE(2,(#29355,#29356,#29357,#29358,#29359,#29360,#29361,#29362,
#29363,#29364,#29365,#29366,#29367),.UNSPECIFIED.,.F.,.F.)
B_SPLINE_CURVE_WITH_KNOTS((3,2,2,2,2,2,3),(0.325,0.333333333333334,0.341666666666667,
0.35,0.358333333333334,0.366666666666666,0.375),.UNSPECIFIED.)
CURVE()
GEOMETRIC_REPRESENTATION_ITEM()
RATIONAL_B_SPLINE_CURVE((1.,0.866025403784439,1.,0.866025403784439,1.,0.866025403784439,
1.,0.866025403784439,1.,0.866025403784439,1.,0.866025403784439,1.))
REPRESENTATION_ITEM('')
);
#87=(
BOUNDED_CURVE()
B_SPLINE_CURVE(2,(#29368,#29369,#29370,#29371,#29372,#29373,#29374,#29375,
#29376,#29377,#29378,#29379,#29380),.UNSPECIFIED.,.F.,.F.)
B_SPLINE_CURVE_WITH_KNOTS((3,2,2,2,2,2,3),(0.325,0.333333333333334,0.341666666666667,
0.35,0.358333333333334,0.366666666666666,0.375),.UNSPECIFIED.)
CURVE()
GEOMETRIC_REPRESENTATION_ITEM()
RATIONAL_B_SPLINE_CURVE((1.,0.866025403784439,1.,0.866025403784439,1.,0.866025403784439,
1.,0.866025403784439,1.,0.866025403784439,1.,0.866025403784439,1.))
REPRESENTATION_ITEM('')
);
#88=(
BOUNDED_CURVE()
B_SPLINE_CURVE(2,(#29385,#29386,#29387,#29388,#29389,#29390,#29391,#29392,
#29393,#29394,#29395,#29396,#29397),.UNSPECIFIED.,.F.,.F.)
B_SPLINE_CURVE_WITH_KNOTS((3,2,2,2,2,2,3),(0.275,0.283333333333334,0.291666666666667,
0.3,0.308333333333334,0.316666666666666,0.325),.UNSPECIFIED.)
CURVE()
GEOMETRIC_REPRESENTATION_ITEM()
RATIONAL_B_SPLINE_CURVE((1.,0.866025403784439,1.,0.866025403784439,1.,0.866025403784439,
1.,0.866025403784439,1.,0.866025403784439,1.,0.866025403784439,1.))
REPRESENTATION_ITEM('')
);
#89=(
BOUNDED_CURVE()
B_SPLINE_CURVE(2,(#29398,#29399,#29400,#29401,#29402,#29403,#29404,#29405,
#29406,#29407,#29408,#29409,#29410),.UNSPECIFIED.,.F.,.F.)
B_SPLINE_CURVE_WITH_KNOTS((3,2,2,2,2,2,3),(0.275,0.283333333333334,0.291666666666667,
0.3,0.308333333333334,0.316666666666666,0.325),.UNSPECIFIED.)
CURVE()
GEOMETRIC_REPRESENTATION_ITEM()
RATIONAL_B_SPLINE_CURVE((1.,0.866025403784439,1.,0.866025403784439,1.,0.866025403784439,
1.,0.866025403784439,1.,0.866025403784439,1.,0.866025403784439,1.))
REPRESENTATION_ITEM('')
);
#90=(
BOUNDED_CURVE()
B_SPLINE_CURVE(2,(#29415,#29416,#29417,#29418,#29419,#29420,#29421,#29422,
#29423,#29424,#29425,#29426,#29427),.UNSPECIFIED.,.F.,.F.)
B_SPLINE_CURVE_WITH_KNOTS((3,2,2,2,2,2,3),(0.225,0.233333333333334,0.241666666666667,
0.25,0.258333333333334,0.266666666666666,0.275),.UNSPECIFIED.)
CURVE()
GEOMETRIC_REPRESENTATION_ITEM()
RATIONAL_B_SPLINE_CURVE((1.,0.866025403784439,1.,0.866025403784439,1.,0.866025403784439,
1.,0.866025403784439,1.,0.866025403784439,1.,0.866025403784439,1.))
REPRESENTATION_ITEM('')
);
#91=(
BOUNDED_CURVE()
B_SPLINE_CURVE(2,(#29428,#29429,#29430,#29431,#29432,#29433,#29434,#29435,
#29436,#29437,#29438,#29439,#29440),.UNSPECIFIED.,.F.,.F.)
B_SPLINE_CURVE_WITH_KNOTS((3,2,2,2,2,2,3),(0.225,0.233333333333334,0.241666666666667,
0.25,0.258333333333334,0.266666666666666,0.275),.UNSPECIFIED.)
CURVE()
GEOMETRIC_REPRESENTATION_ITEM()
RATIONAL_B_SPLINE_CURVE((1.,0.866025403784439,1.,0.866025403784439,1.,0.866025403784439,
1.,0.866025403784439,1.,0.866025403784439,1.,0.866025403784439,1.))
REPRESENTATION_ITEM('')
);
#92=(
BOUNDED_CURVE()
B_SPLINE_CURVE(2,(#29445,#29446,#29447,#29448,#29449,#29450,#29451,#29452,
#29453,#29454,#29455,#29456,#29457),.UNSPECIFIED.,.F.,.F.)
B_SPLINE_CURVE_WITH_KNOTS((3,2,2,2,2,2,3),(0.175,0.183333333333334,0.191666666666667,
0.2,0.208333333333334,0.216666666666667,0.225),.UNSPECIFIED.)
CURVE()
GEOMETRIC_REPRESENTATION_ITEM()
RATIONAL_B_SPLINE_CURVE((1.,0.866025403784439,1.,0.866025403784439,1.,0.866025403784439,
1.,0.866025403784439,1.,0.866025403784439,1.,0.866025403784439,1.))
REPRESENTATION_ITEM('')
);
#93=(
BOUNDED_CURVE()
B_SPLINE_CURVE(2,(#29458,#29459,#29460,#29461,#29462,#29463,#29464,#29465,
#29466,#29467,#29468,#29469,#29470),.UNSPECIFIED.,.F.,.F.)
B_SPLINE_CURVE_WITH_KNOTS((3,2,2,2,2,2,3),(0.175,0.183333333333334,0.191666666666667,
0.2,0.208333333333334,0.216666666666667,0.225),.UNSPECIFIED.)
CURVE()
GEOMETRIC_REPRESENTATION_ITEM()
RATIONAL_B_SPLINE_CURVE((1.,0.866025403784439,1.,0.866025403784439,1.,0.866025403784439,
1.,0.866025403784439,1.,0.866025403784439,1.,0.866025403784439,1.))
REPRESENTATION_ITEM('')
);
#94=(
BOUNDED_CURVE()
B_SPLINE_CURVE(2,(#29475,#29476,#29477,#29478,#29479,#29480,#29481,#29482,
#29483,#29484,#29485,#29486,#29487),.UNSPECIFIED.,.F.,.F.)
B_SPLINE_CURVE_WITH_KNOTS((3,2,2,2,2,2,3),(0.125,0.133333333333333,0.141666666666667,
0.15,0.158333333333333,0.166666666666667,0.175),.UNSPECIFIED.)
CURVE()
GEOMETRIC_REPRESENTATION_ITEM()
RATIONAL_B_SPLINE_CURVE((1.,0.866025403784439,1.,0.866025403784439,1.,0.866025403784439,
1.,0.866025403784439,1.,0.866025403784439,1.,0.866025403784439,1.))
REPRESENTATION_ITEM('')
);
#95=(
BOUNDED_CURVE()
B_SPLINE_CURVE(2,(#29488,#29489,#29490,#29491,#29492,#29493,#29494,#29495,
#29496,#29497,#29498,#29499,#29500),.UNSPECIFIED.,.F.,.F.)
B_SPLINE_CURVE_WITH_KNOTS((3,2,2,2,2,2,3),(0.125,0.133333333333333,0.141666666666667,
0.15,0.158333333333333,0.166666666666667,0.175),.UNSPECIFIED.)
CURVE()
GEOMETRIC_REPRESENTATION_ITEM()
RATIONAL_B_SPLINE_CURVE((1.,0.866025403784439,1.,0.866025403784439,1.,0.866025403784439,
1.,0.866025403784439,1.,0.866025403784439,1.,0.866025403784439,1.))
REPRESENTATION_ITEM('')
);
#96=(
BOUNDED_CURVE()
B_SPLINE_CURVE(2,(#29505,#29506,#29507,#29508,#29509,#29510,#29511,#29512,
#29513,#29514,#29515,#29516,#29517),.UNSPECIFIED.,.F.,.F.)
B_SPLINE_CURVE_WITH_KNOTS((3,2,2,2,2,2,3),(0.075,0.0833333333333333,0.0916666666666667,
0.1,0.108333333333333,0.116666666666667,0.125),.UNSPECIFIED.)
CURVE()
GEOMETRIC_REPRESENTATION_ITEM()
RATIONAL_B_SPLINE_CURVE((1.,0.866025403784439,1.,0.866025403784439,1.,0.866025403784439,
1.,0.866025403784439,1.,0.866025403784439,1.,0.866025403784439,1.))
REPRESENTATION_ITEM('')
);
#97=(
BOUNDED_CURVE()
B_SPLINE_CURVE(2,(#29518,#29519,#29520,#29521,#29522,#29523,#29524,#29525,
#29526,#29527,#29528,#29529,#29530),.UNSPECIFIED.,.F.,.F.)
B_SPLINE_CURVE_WITH_KNOTS((3,2,2,2,2,2,3),(0.075,0.0833333333333333,0.0916666666666667,
0.1,0.108333333333333,0.116666666666667,0.125),.UNSPECIFIED.)
CURVE()
GEOMETRIC_REPRESENTATION_ITEM()
RATIONAL_B_SPLINE_CURVE((1.,0.866025403784439,1.,0.866025403784439,1.,0.866025403784439,
1.,0.866025403784439,1.,0.866025403784439,1.,0.866025403784439,1.))
REPRESENTATION_ITEM('')
);
#98=(
BOUNDED_CURVE()
B_SPLINE_CURVE(2,(#29536,#29537,#29538,#29539,#29540,#29541,#29542),
 .UNSPECIFIED.,.F.,.F.)
B_SPLINE_CURVE_WITH_KNOTS((3,2,2,3),(0.,0.00833333333333333,0.0166666666666666,
0.025),.UNSPECIFIED.)
CURVE()
GEOMETRIC_REPRESENTATION_ITEM()
RATIONAL_B_SPLINE_CURVE((1.,0.866025403784439,1.,0.866025403784439,1.,0.866025403784439,
1.))
REPRESENTATION_ITEM('')
);
#99=(
BOUNDED_CURVE()
B_SPLINE_CURVE(2,(#29545,#29546,#29547,#29548,#29549,#29550,#29551),
 .UNSPECIFIED.,.F.,.F.)
B_SPLINE_CURVE_WITH_KNOTS((3,2,2,3),(0.,0.00833333333333333,0.0166666666666666,
0.025),.UNSPECIFIED.)
CURVE()
GEOMETRIC_REPRESENTATION_ITEM()
RATIONAL_B_SPLINE_CURVE((1.,0.866025403784439,1.,0.866025403784439,1.,0.866025403784439,
1.))
REPRESENTATION_ITEM('')
);
#100=(
BOUNDED_CURVE()
B_SPLINE_CURVE(2,(#29776,#29777,#29778,#29779,#29780,#29781,#29782,#29783,
#29784),.UNSPECIFIED.,.F.,.F.)
B_SPLINE_CURVE_WITH_KNOTS((3,2,2,2,3),(0.9375,0.953125,0.96875,0.984375,
1.),.UNSPECIFIED.)
CURVE()
GEOMETRIC_REPRESENTATION_ITEM()
RATIONAL_B_SPLINE_CURVE((1.,0.923879532511287,1.,0.923879532511287,1.,0.923879532511287,
1.,0.923879532511287,1.))
REPRESENTATION_ITEM('')
);
#101=(
BOUNDED_CURVE()
B_SPLINE_CURVE(2,(#29787,#29788,#29789,#29790,#29791,#29792,#29793,#29794,
#29795),.UNSPECIFIED.,.F.,.F.)
B_SPLINE_CURVE_WITH_KNOTS((3,2,2,2,3),(0.9375,0.953125,0.96875,0.984375,
1.),.UNSPECIFIED.)
CURVE()
GEOMETRIC_REPRESENTATION_ITEM()
RATIONAL_B_SPLINE_CURVE((1.,0.923879532511287,1.,0.923879532511287,1.,0.923879532511287,
1.,0.923879532511287,1.))
REPRESENTATION_ITEM('')
);
#102=(
BOUNDED_CURVE()
B_SPLINE_CURVE(2,(#29800,#29801,#29802,#29803,#29804,#29805,#29806,#29807,
#29808,#29809,#29810,#29811,#29812,#29813,#29814,#29815,#29816),
 .UNSPECIFIED.,.F.,.F.)
B_SPLINE_CURVE_WITH_KNOTS((3,2,2,2,2,2,2,2,3),(0.8125,0.828125,0.84375,
0.859375,0.875,0.890625,0.90625,0.921875,0.9375),.UNSPECIFIED.)
CURVE()
GEOMETRIC_REPRESENTATION_ITEM()
RATIONAL_B_SPLINE_CURVE((1.,0.923879532511287,1.,0.923879532511287,1.,0.923879532511287,
1.,0.923879532511287,1.,0.923879532511287,1.,0.923879532511287,1.,0.923879532511287,
1.,0.923879532511287,1.))
REPRESENTATION_ITEM('')
);
#103=(
BOUNDED_CURVE()
B_SPLINE_CURVE(2,(#29817,#29818,#29819,#29820,#29821,#29822,#29823,#29824,
#29825,#29826,#29827,#29828,#29829,#29830,#29831,#29832,#29833),
 .UNSPECIFIED.,.F.,.F.)
B_SPLINE_CURVE_WITH_KNOTS((3,2,2,2,2,2,2,2,3),(0.8125,0.828125,0.84375,
0.859375,0.875,0.890625,0.90625,0.921875,0.9375),.UNSPECIFIED.)
CURVE()
GEOMETRIC_REPRESENTATION_ITEM()
RATIONAL_B_SPLINE_CURVE((1.,0.923879532511287,1.,0.923879532511287,1.,0.923879532511287,
1.,0.923879532511287,1.,0.923879532511287,1.,0.923879532511287,1.,0.923879532511287,
1.,0.923879532511287,1.))
REPRESENTATION_ITEM('')
);
#104=(
BOUNDED_CURVE()
B_SPLINE_CURVE(2,(#29838,#29839,#29840,#29841,#29842,#29843,#29844,#29845,
#29846,#29847,#29848,#29849,#29850,#29851,#29852,#29853,#29854),
 .UNSPECIFIED.,.F.,.F.)
B_SPLINE_CURVE_WITH_KNOTS((3,2,2,2,2,2,2,2,3),(0.6875,0.703125,0.71875,
0.734375,0.75,0.765625,0.78125,0.796875,0.8125),.UNSPECIFIED.)
CURVE()
GEOMETRIC_REPRESENTATION_ITEM()
RATIONAL_B_SPLINE_CURVE((1.,0.923879532511287,1.,0.923879532511287,1.,0.923879532511287,
1.,0.923879532511287,1.,0.923879532511287,1.,0.923879532511287,1.,0.923879532511287,
1.,0.923879532511287,1.))
REPRESENTATION_ITEM('')
);
#105=(
BOUNDED_CURVE()
B_SPLINE_CURVE(2,(#29855,#29856,#29857,#29858,#29859,#29860,#29861,#29862,
#29863,#29864,#29865,#29866,#29867,#29868,#29869,#29870,#29871),
 .UNSPECIFIED.,.F.,.F.)
B_SPLINE_CURVE_WITH_KNOTS((3,2,2,2,2,2,2,2,3),(0.6875,0.703125,0.71875,
0.734375,0.75,0.765625,0.78125,0.796875,0.8125),.UNSPECIFIED.)
CURVE()
GEOMETRIC_REPRESENTATION_ITEM()
RATIONAL_B_SPLINE_CURVE((1.,0.923879532511287,1.,0.923879532511287,1.,0.923879532511287,
1.,0.923879532511287,1.,0.923879532511287,1.,0.923879532511287,1.,0.923879532511287,
1.,0.923879532511287,1.))
REPRESENTATION_ITEM('')
);
#106=(
BOUNDED_CURVE()
B_SPLINE_CURVE(2,(#29876,#29877,#29878,#29879,#29880,#29881,#29882,#29883,
#29884,#29885,#29886,#29887,#29888,#29889,#29890,#29891,#29892),
 .UNSPECIFIED.,.F.,.F.)
B_SPLINE_CURVE_WITH_KNOTS((3,2,2,2,2,2,2,2,3),(0.5625,0.578125,0.59375,
0.609375,0.625,0.640625,0.65625,0.671875,0.6875),.UNSPECIFIED.)
CURVE()
GEOMETRIC_REPRESENTATION_ITEM()
RATIONAL_B_SPLINE_CURVE((1.,0.923879532511287,1.,0.923879532511287,1.,0.923879532511287,
1.,0.923879532511287,1.,0.923879532511287,1.,0.923879532511287,1.,0.923879532511287,
1.,0.923879532511287,1.))
REPRESENTATION_ITEM('')
);
#107=(
BOUNDED_CURVE()
B_SPLINE_CURVE(2,(#29893,#29894,#29895,#29896,#29897,#29898,#29899,#29900,
#29901,#29902,#29903,#29904,#29905,#29906,#29907,#29908,#29909),
 .UNSPECIFIED.,.F.,.F.)
B_SPLINE_CURVE_WITH_KNOTS((3,2,2,2,2,2,2,2,3),(0.5625,0.578125,0.59375,
0.609375,0.625,0.640625,0.65625,0.671875,0.6875),.UNSPECIFIED.)
CURVE()
GEOMETRIC_REPRESENTATION_ITEM()
RATIONAL_B_SPLINE_CURVE((1.,0.923879532511287,1.,0.923879532511287,1.,0.923879532511287,
1.,0.923879532511287,1.,0.923879532511287,1.,0.923879532511287,1.,0.923879532511287,
1.,0.923879532511287,1.))
REPRESENTATION_ITEM('')
);
#108=(
BOUNDED_CURVE()
B_SPLINE_CURVE(2,(#29914,#29915,#29916,#29917,#29918,#29919,#29920,#29921,
#29922,#29923,#29924,#29925,#29926,#29927,#29928,#29929,#29930),
 .UNSPECIFIED.,.F.,.F.)
B_SPLINE_CURVE_WITH_KNOTS((3,2,2,2,2,2,2,2,3),(0.4375,0.453125,0.46875,
0.484375,0.5,0.515625,0.53125,0.546875,0.5625),.UNSPECIFIED.)
CURVE()
GEOMETRIC_REPRESENTATION_ITEM()
RATIONAL_B_SPLINE_CURVE((1.,0.923879532511287,1.,0.923879532511287,1.,0.923879532511287,
1.,0.923879532511287,1.,0.923879532511287,1.,0.923879532511287,1.,0.923879532511287,
1.,0.923879532511287,1.))
REPRESENTATION_ITEM('')
);
#109=(
BOUNDED_CURVE()
B_SPLINE_CURVE(2,(#29931,#29932,#29933,#29934,#29935,#29936,#29937,#29938,
#29939,#29940,#29941,#29942,#29943,#29944,#29945,#29946,#29947),
 .UNSPECIFIED.,.F.,.F.)
B_SPLINE_CURVE_WITH_KNOTS((3,2,2,2,2,2,2,2,3),(0.4375,0.453125,0.46875,
0.484375,0.5,0.515625,0.53125,0.546875,0.5625),.UNSPECIFIED.)
CURVE()
GEOMETRIC_REPRESENTATION_ITEM()
RATIONAL_B_SPLINE_CURVE((1.,0.923879532511287,1.,0.923879532511287,1.,0.923879532511287,
1.,0.923879532511287,1.,0.923879532511287,1.,0.923879532511287,1.,0.923879532511287,
1.,0.923879532511287,1.))
REPRESENTATION_ITEM('')
);
#110=(
BOUNDED_CURVE()
B_SPLINE_CURVE(2,(#29952,#29953,#29954,#29955,#29956,#29957,#29958,#29959,
#29960,#29961,#29962,#29963,#29964,#29965,#29966,#29967,#29968),
 .UNSPECIFIED.,.F.,.F.)
B_SPLINE_CURVE_WITH_KNOTS((3,2,2,2,2,2,2,2,3),(0.3125,0.328125,0.34375,
0.359375,0.375,0.390625,0.40625,0.421875,0.4375),.UNSPECIFIED.)
CURVE()
GEOMETRIC_REPRESENTATION_ITEM()
RATIONAL_B_SPLINE_CURVE((1.,0.923879532511287,1.,0.923879532511287,1.,0.923879532511287,
1.,0.923879532511287,1.,0.923879532511287,1.,0.923879532511287,1.,0.923879532511287,
1.,0.923879532511287,1.))
REPRESENTATION_ITEM('')
);
#111=(
BOUNDED_CURVE()
B_SPLINE_CURVE(2,(#29969,#29970,#29971,#29972,#29973,#29974,#29975,#29976,
#29977,#29978,#29979,#29980,#29981,#29982,#29983,#29984,#29985),
 .UNSPECIFIED.,.F.,.F.)
B_SPLINE_CURVE_WITH_KNOTS((3,2,2,2,2,2,2,2,3),(0.3125,0.328125,0.34375,
0.359375,0.375,0.390625,0.40625,0.421875,0.4375),.UNSPECIFIED.)
CURVE()
GEOMETRIC_REPRESENTATION_ITEM()
RATIONAL_B_SPLINE_CURVE((1.,0.923879532511287,1.,0.923879532511287,1.,0.923879532511287,
1.,0.923879532511287,1.,0.923879532511287,1.,0.923879532511287,1.,0.923879532511287,
1.,0.923879532511287,1.))
REPRESENTATION_ITEM('')
);
#112=(
BOUNDED_CURVE()
B_SPLINE_CURVE(2,(#29990,#29991,#29992,#29993,#29994,#29995,#29996,#29997,
#29998,#29999,#30000,#30001,#30002,#30003,#30004,#30005,#30006),
 .UNSPECIFIED.,.F.,.F.)
B_SPLINE_CURVE_WITH_KNOTS((3,2,2,2,2,2,2,2,3),(0.1875,0.203125,0.21875,
0.234375,0.25,0.265625,0.28125,0.296875,0.3125),.UNSPECIFIED.)
CURVE()
GEOMETRIC_REPRESENTATION_ITEM()
RATIONAL_B_SPLINE_CURVE((1.,0.923879532511287,1.,0.923879532511287,1.,0.923879532511287,
1.,0.923879532511287,1.,0.923879532511287,1.,0.923879532511287,1.,0.923879532511287,
1.,0.923879532511287,1.))
REPRESENTATION_ITEM('')
);
#113=(
BOUNDED_CURVE()
B_SPLINE_CURVE(2,(#30007,#30008,#30009,#30010,#30011,#30012,#30013,#30014,
#30015,#30016,#30017,#30018,#30019,#30020,#30021,#30022,#30023),
 .UNSPECIFIED.,.F.,.F.)
B_SPLINE_CURVE_WITH_KNOTS((3,2,2,2,2,2,2,2,3),(0.1875,0.203125,0.21875,
0.234375,0.25,0.265625,0.28125,0.296875,0.3125),.UNSPECIFIED.)
CURVE()
GEOMETRIC_REPRESENTATION_ITEM()
RATIONAL_B_SPLINE_CURVE((1.,0.923879532511287,1.,0.923879532511287,1.,0.923879532511287,
1.,0.923879532511287,1.,0.923879532511287,1.,0.923879532511287,1.,0.923879532511287,
1.,0.923879532511287,1.))
REPRESENTATION_ITEM('')
);
#114=(
BOUNDED_CURVE()
B_SPLINE_CURVE(2,(#30028,#30029,#30030,#30031,#30032,#30033,#30034,#30035,
#30036,#30037,#30038,#30039,#30040,#30041,#30042,#30043,#30044),
 .UNSPECIFIED.,.F.,.F.)
B_SPLINE_CURVE_WITH_KNOTS((3,2,2,2,2,2,2,2,3),(0.0625,0.078125,0.09375,
0.109375,0.125,0.140625,0.15625,0.171875,0.1875),.UNSPECIFIED.)
CURVE()
GEOMETRIC_REPRESENTATION_ITEM()
RATIONAL_B_SPLINE_CURVE((1.,0.923879532511287,1.,0.923879532511287,1.,0.923879532511287,
1.,0.923879532511287,1.,0.923879532511287,1.,0.923879532511287,1.,0.923879532511287,
1.,0.923879532511287,1.))
REPRESENTATION_ITEM('')
);
#115=(
BOUNDED_CURVE()
B_SPLINE_CURVE(2,(#30045,#30046,#30047,#30048,#30049,#30050,#30051,#30052,
#30053,#30054,#30055,#30056,#30057,#30058,#30059,#30060,#30061),
 .UNSPECIFIED.,.F.,.F.)
B_SPLINE_CURVE_WITH_KNOTS((3,2,2,2,2,2,2,2,3),(0.0625,0.078125,0.09375,
0.109375,0.125,0.140625,0.15625,0.171875,0.1875),.UNSPECIFIED.)
CURVE()
GEOMETRIC_REPRESENTATION_ITEM()
RATIONAL_B_SPLINE_CURVE((1.,0.923879532511287,1.,0.923879532511287,1.,0.923879532511287,
1.,0.923879532511287,1.,0.923879532511287,1.,0.923879532511287,1.,0.923879532511287,
1.,0.923879532511287,1.))
REPRESENTATION_ITEM('')
);
#116=(
BOUNDED_CURVE()
B_SPLINE_CURVE(2,(#30407,#30408,#30409),.UNSPECIFIED.,.F.,.F.)
B_SPLINE_CURVE_WITH_KNOTS((3,3),(-2.29029703823251,-1.6630480152671),
 .UNSPECIFIED.)
CURVE()
GEOMETRIC_REPRESENTATION_ITEM()
RATIONAL_B_SPLINE_CURVE((1.40847966848734,1.4295768207167,1.40847966848734))
REPRESENTATION_ITEM('')
);
#117=(
BOUNDED_CURVE()
B_SPLINE_CURVE(2,(#30414,#30415,#30416),.UNSPECIFIED.,.F.,.F.)
B_SPLINE_CURVE_WITH_KNOTS((3,3),(-0.660669052460662,-0.357639202089822),
 .UNSPECIFIED.)
CURVE()
GEOMETRIC_REPRESENTATION_ITEM()
RATIONAL_B_SPLINE_CURVE((1.03886559867011,1.03696952671266,1.02863628649672))
REPRESENTATION_ITEM('')
);
#118=(
BOUNDED_CURVE()
B_SPLINE_CURVE(2,(#30422,#30423,#30424),.UNSPECIFIED.,.F.,.F.)
B_SPLINE_CURVE_WITH_KNOTS((3,3),(-1.14221416870175,-0.839184318331155),
 .UNSPECIFIED.)
CURVE()
GEOMETRIC_REPRESENTATION_ITEM()
RATIONAL_B_SPLINE_CURVE((1.02863628649616,1.03696952671193,1.03886559866935))
REPRESENTATION_ITEM('')
);
#119=(
BOUNDED_CURVE()
B_SPLINE_CURVE(2,(#30440,#30441,#30442),.UNSPECIFIED.,.F.,.F.)
B_SPLINE_CURVE_WITH_KNOTS((3,3),(-1.14221416870072,-0.839184318329676),
 .UNSPECIFIED.)
CURVE()
GEOMETRIC_REPRESENTATION_ITEM()
RATIONAL_B_SPLINE_CURVE((1.02863628649697,1.03696952671296,1.0388655986704))
REPRESENTATION_ITEM('')
);
#120=(
BOUNDED_CURVE()
B_SPLINE_CURVE(2,(#30449,#30450,#30451),.UNSPECIFIED.,.F.,.F.)
B_SPLINE_CURVE_WITH_KNOTS((3,3),(-2.29029703823251,-1.6630480152671),
 .UNSPECIFIED.)
CURVE()
GEOMETRIC_REPRESENTATION_ITEM()
RATIONAL_B_SPLINE_CURVE((1.40847966848733,1.4295768207167,1.40847966848733))
REPRESENTATION_ITEM('')
);
#121=(
BOUNDED_CURVE()
B_SPLINE_CURVE(2,(#30455,#30456,#30457),.UNSPECIFIED.,.F.,.F.)
B_SPLINE_CURVE_WITH_KNOTS((3,3),(-0.660669052461382,-0.357639202090536),
 .UNSPECIFIED.)
CURVE()
GEOMETRIC_REPRESENTATION_ITEM()
RATIONAL_B_SPLINE_CURVE((1.03886559866973,1.03696952671232,1.02863628649648))
REPRESENTATION_ITEM('')
);
#122=(
BOUNDED_CURVE()
B_SPLINE_CURVE(2,(#30473,#30474,#30475),.UNSPECIFIED.,.F.,.F.)
B_SPLINE_CURVE_WITH_KNOTS((3,3),(-1.14221416870089,-0.839184318330394),
 .UNSPECIFIED.)
CURVE()
GEOMETRIC_REPRESENTATION_ITEM()
RATIONAL_B_SPLINE_CURVE((1.02863628649558,1.03696952671116,1.03886559866852))
REPRESENTATION_ITEM('')
);
#123=(
BOUNDED_CURVE()
B_SPLINE_CURVE(2,(#30482,#30483,#30484),.UNSPECIFIED.,.F.,.F.)
B_SPLINE_CURVE_WITH_KNOTS((3,3),(-2.29029703823246,-1.66304801526705),
 .UNSPECIFIED.)
CURVE()
GEOMETRIC_REPRESENTATION_ITEM()
RATIONAL_B_SPLINE_CURVE((1.40847966848734,1.4295768207167,1.40847966848733))
REPRESENTATION_ITEM('')
);
#124=(
BOUNDED_CURVE()
B_SPLINE_CURVE(2,(#30488,#30489,#30490),.UNSPECIFIED.,.F.,.F.)
B_SPLINE_CURVE_WITH_KNOTS((3,3),(-0.660669052461842,-0.35763920209058),
 .UNSPECIFIED.)
CURVE()
GEOMETRIC_REPRESENTATION_ITEM()
RATIONAL_B_SPLINE_CURVE((1.03886559867121,1.03696952671373,1.02863628649756))
REPRESENTATION_ITEM('')
);
#125=(
BOUNDED_CURVE()
B_SPLINE_CURVE(2,(#30508,#30509,#30510),.UNSPECIFIED.,.F.,.F.)
B_SPLINE_CURVE_WITH_KNOTS((3,3),(-1.14221416870064,-0.839184318329342),
 .UNSPECIFIED.)
CURVE()
GEOMETRIC_REPRESENTATION_ITEM()
RATIONAL_B_SPLINE_CURVE((1.0286362864976,1.03696952671377,1.03886559867125))
REPRESENTATION_ITEM('')
);
#126=(
BOUNDED_CURVE()
B_SPLINE_CURVE(2,(#30518,#30519,#30520),.UNSPECIFIED.,.F.,.F.)
B_SPLINE_CURVE_WITH_KNOTS((3,3),(-2.29029703823249,-1.97667252674982),
 .UNSPECIFIED.)
CURVE()
GEOMETRIC_REPRESENTATION_ITEM()
RATIONAL_B_SPLINE_CURVE((1.40847966848735,1.41902824460203,1.41902824460203))
REPRESENTATION_ITEM('')
);
#127=(
BOUNDED_CURVE()
B_SPLINE_CURVE(2,(#30521,#30522,#30523),.UNSPECIFIED.,.F.,.F.)
B_SPLINE_CURVE_WITH_KNOTS((3,3),(-1.97667252674982,-1.66304801526709),
 .UNSPECIFIED.)
CURVE()
GEOMETRIC_REPRESENTATION_ITEM()
RATIONAL_B_SPLINE_CURVE((1.41902824460203,1.41902824460203,1.40847966848735))
REPRESENTATION_ITEM('')
);
#128=(
BOUNDED_CURVE()
B_SPLINE_CURVE(2,(#30527,#30528,#30529),.UNSPECIFIED.,.F.,.F.)
B_SPLINE_CURVE_WITH_KNOTS((3,3),(-0.660669052460473,-0.357639202089695),
 .UNSPECIFIED.)
CURVE()
GEOMETRIC_REPRESENTATION_ITEM()
RATIONAL_B_SPLINE_CURVE((1.03886559866983,1.03696952671239,1.02863628649651))
REPRESENTATION_ITEM('')
);
#129=(
BOUNDED_CURVE()
B_SPLINE_CURVE(2,(#30852,#30853,#30854,#30855,#30856,#30857,#30858,#30859,
#30860),.UNSPECIFIED.,.F.,.F.)
B_SPLINE_CURVE_WITH_KNOTS((3,2,2,2,3),(0.,0.015625,0.03125,0.046875,0.0625),
 .UNSPECIFIED.)
CURVE()
GEOMETRIC_REPRESENTATION_ITEM()
RATIONAL_B_SPLINE_CURVE((1.,0.923879532511287,1.,0.923879532511287,1.,0.923879532511287,
1.,0.923879532511287,1.))
REPRESENTATION_ITEM('')
);
#130=(
BOUNDED_CURVE()
B_SPLINE_CURVE(2,(#30864,#30865,#30866,#30867,#30868,#30869,#30870,#30871,
#30872,#30873,#30874,#30875,#30876,#30877,#30878),.UNSPECIFIED.,.F.,.F.)
B_SPLINE_CURVE_WITH_KNOTS((3,2,2,2,2,2,2,3),(0.890625000369527,0.90625,
0.921875,0.9375,0.953125,0.96875,0.984375,1.),.UNSPECIFIED.)
CURVE()
GEOMETRIC_REPRESENTATION_ITEM()
RATIONAL_B_SPLINE_CURVE((0.999999996399544,0.923879534311515,1.,0.923879532511287,
1.,0.923879532511287,1.,0.923879532511287,1.,0.923879532511287,1.,0.923879532511287,
1.,0.923879532511287,1.))
REPRESENTATION_ITEM('')
);
#131=(
BOUNDED_CURVE()
B_SPLINE_CURVE(2,(#31184,#31185,#31186,#31187,#31188,#31189,#31190,#31191,
#31192),.UNSPECIFIED.,.F.,.F.)
B_SPLINE_CURVE_WITH_KNOTS((3,2,2,2,3),(0.,0.015625,0.03125,0.046875,0.0625),
 .UNSPECIFIED.)
CURVE()
GEOMETRIC_REPRESENTATION_ITEM()
RATIONAL_B_SPLINE_CURVE((1.,0.923879532511287,1.,0.923879532511287,1.,0.923879532511287,
1.,0.923879532511287,1.))
REPRESENTATION_ITEM('')
);
#132=(
BOUNDED_CURVE()
B_SPLINE_CURVE(2,(#32374,#32375,#32376,#32377,#32378,#32379,#32380,#32381,
#32382),.UNSPECIFIED.,.F.,.F.)
B_SPLINE_CURVE_WITH_KNOTS((3,2,2,2,3),(0.949015774239672,0.95,0.958333333333333,
0.966666666666667,0.975),.UNSPECIFIED.)
CURVE()
GEOMETRIC_REPRESENTATION_ITEM()
RATIONAL_B_SPLINE_CURVE((0.972090999933038,0.984176650141011,1.,0.866025403784439,
1.,0.866025403784439,1.,0.866025403784439,1.))
REPRESENTATION_ITEM('')
);
#133=(
BOUNDED_CURVE()
B_SPLINE_CURVE(2,(#32384,#32385,#32386,#32387,#32388,#32389,#32390,#32391,
#32392,#32393,#32394,#32395,#32396),.UNSPECIFIED.,.F.,.F.)
B_SPLINE_CURVE_WITH_KNOTS((3,2,2,2,2,2,3),(0.025,0.0333333333333333,0.0416666666666667,
0.05,0.0583333333333333,0.0666666666666667,0.075),.UNSPECIFIED.)
CURVE()
GEOMETRIC_REPRESENTATION_ITEM()
RATIONAL_B_SPLINE_CURVE((1.,0.866025403784439,1.,0.866025403784439,1.,0.866025403784439,
1.,0.866025403784439,1.,0.866025403784439,1.,0.866025403784439,1.))
REPRESENTATION_ITEM('')
);
#134=(
BOUNDED_CURVE()
B_SPLINE_CURVE(2,(#32398,#32399,#32400,#32401,#32402,#32403,#32404,#32405,
#32406,#32407,#32408,#32409,#32410),.UNSPECIFIED.,.F.,.F.)
B_SPLINE_CURVE_WITH_KNOTS((3,2,2,2,2,2,3),(0.025,0.0333333333333333,0.0416666666666667,
0.05,0.0583333333333333,0.0666666666666667,0.075),.UNSPECIFIED.)
CURVE()
GEOMETRIC_REPRESENTATION_ITEM()
RATIONAL_B_SPLINE_CURVE((1.,0.866025403784439,1.,0.866025403784439,1.,0.866025403784439,
1.,0.866025403784439,1.,0.866025403784439,1.,0.866025403784439,1.))
REPRESENTATION_ITEM('')
);
#135=(
BOUNDED_CURVE()
B_SPLINE_CURVE(2,(#32932,#32933,#32934,#32935,#32936,#32937,#32938,#32939,
#32940),.UNSPECIFIED.,.F.,.F.)
B_SPLINE_CURVE_WITH_KNOTS((3,2,2,2,3),(0.,0.00833333333333333,0.0166666666666666,
0.025,0.0286105917769561),.UNSPECIFIED.)
CURVE()
GEOMETRIC_REPRESENTATION_ITEM()
RATIONAL_B_SPLINE_CURVE((1.,0.866025403784439,1.,0.866025403784439,1.,0.866025403784439,
1.,0.941952690949969,0.934205814715252))
REPRESENTATION_ITEM('')
);
#136=(
BOUNDED_CURVE()
B_SPLINE_CURVE(2,(#34733,#34734,#34735,#34736,#34737,#34738,#34739),
 .UNSPECIFIED.,.F.,.F.)
B_SPLINE_CURVE_WITH_KNOTS((3,2,2,3),(0.964285714285714,0.976190476190476,
0.988095238095238,1.),.UNSPECIFIED.)
CURVE()
GEOMETRIC_REPRESENTATION_ITEM()
RATIONAL_B_SPLINE_CURVE((1.,0.866025403784439,1.,0.866025403784439,1.,0.866025403784439,
1.))
REPRESENTATION_ITEM('')
);
#137=(
BOUNDED_CURVE()
B_SPLINE_CURVE(2,(#34742,#34743,#34744,#34745,#34746,#34747,#34748),
 .UNSPECIFIED.,.F.,.F.)
B_SPLINE_CURVE_WITH_KNOTS((3,2,2,3),(0.964285714285714,0.976190476190476,
0.988095238095238,1.),.UNSPECIFIED.)
CURVE()
GEOMETRIC_REPRESENTATION_ITEM()
RATIONAL_B_SPLINE_CURVE((1.,0.866025403784439,1.,0.866025403784439,1.,0.866025403784439,
1.))
REPRESENTATION_ITEM('')
);
#138=(
BOUNDED_CURVE()
B_SPLINE_CURVE(2,(#34753,#34754,#34755,#34756,#34757,#34758,#34759,#34760,
#34761,#34762,#34763,#34764,#34765),.UNSPECIFIED.,.F.,.F.)
B_SPLINE_CURVE_WITH_KNOTS((3,2,2,2,2,2,3),(0.892857142857143,0.904761904761905,
0.916666666666667,0.928571428571429,0.94047619047619,0.952380952380952,
0.964285714285714),.UNSPECIFIED.)
CURVE()
GEOMETRIC_REPRESENTATION_ITEM()
RATIONAL_B_SPLINE_CURVE((1.,0.866025403784439,1.,0.866025403784439,1.,0.866025403784439,
1.,0.866025403784439,1.,0.866025403784439,1.,0.866025403784439,1.))
REPRESENTATION_ITEM('')
);
#139=(
BOUNDED_CURVE()
B_SPLINE_CURVE(2,(#34766,#34767,#34768,#34769,#34770,#34771,#34772,#34773,
#34774,#34775,#34776,#34777,#34778),.UNSPECIFIED.,.F.,.F.)
B_SPLINE_CURVE_WITH_KNOTS((3,2,2,2,2,2,3),(0.892857142857143,0.904761904761905,
0.916666666666667,0.928571428571429,0.94047619047619,0.952380952380952,
0.964285714285714),.UNSPECIFIED.)
CURVE()
GEOMETRIC_REPRESENTATION_ITEM()
RATIONAL_B_SPLINE_CURVE((1.,0.866025403784439,1.,0.866025403784439,1.,0.866025403784439,
1.,0.866025403784439,1.,0.866025403784439,1.,0.866025403784439,1.))
REPRESENTATION_ITEM('')
);
#140=(
BOUNDED_CURVE()
B_SPLINE_CURVE(2,(#34783,#34784,#34785,#34786,#34787,#34788,#34789,#34790,
#34791,#34792,#34793,#34794,#34795),.UNSPECIFIED.,.F.,.F.)
B_SPLINE_CURVE_WITH_KNOTS((3,2,2,2,2,2,3),(0.821428571428572,0.833333333333333,
0.845238095238095,0.857142857142857,0.869047619047619,0.880952380952381,
0.892857142857143),.UNSPECIFIED.)
CURVE()
GEOMETRIC_REPRESENTATION_ITEM()
RATIONAL_B_SPLINE_CURVE((1.,0.866025403784439,1.,0.866025403784439,1.,0.866025403784439,
1.,0.866025403784439,1.,0.866025403784439,1.,0.866025403784439,1.))
REPRESENTATION_ITEM('')
);
#141=(
BOUNDED_CURVE()
B_SPLINE_CURVE(2,(#34796,#34797,#34798,#34799,#34800,#34801,#34802,#34803,
#34804,#34805,#34806,#34807,#34808),.UNSPECIFIED.,.F.,.F.)
B_SPLINE_CURVE_WITH_KNOTS((3,2,2,2,2,2,3),(0.821428571428572,0.833333333333333,
0.845238095238095,0.857142857142857,0.869047619047619,0.880952380952381,
0.892857142857143),.UNSPECIFIED.)
CURVE()
GEOMETRIC_REPRESENTATION_ITEM()
RATIONAL_B_SPLINE_CURVE((1.,0.866025403784439,1.,0.866025403784439,1.,0.866025403784439,
1.,0.866025403784439,1.,0.866025403784439,1.,0.866025403784439,1.))
REPRESENTATION_ITEM('')
);
#142=(
BOUNDED_CURVE()
B_SPLINE_CURVE(2,(#34813,#34814,#34815,#34816,#34817,#34818,#34819,#34820,
#34821,#34822,#34823,#34824,#34825),.UNSPECIFIED.,.F.,.F.)
B_SPLINE_CURVE_WITH_KNOTS((3,2,2,2,2,2,3),(0.75,0.761904761904762,0.773809523809524,
0.785714285714286,0.797619047619048,0.809523809523809,0.821428571428572),
 .UNSPECIFIED.)
CURVE()
GEOMETRIC_REPRESENTATION_ITEM()
RATIONAL_B_SPLINE_CURVE((1.,0.866025403784439,1.,0.866025403784439,1.,0.866025403784439,
1.,0.866025403784439,1.,0.866025403784439,1.,0.866025403784439,1.))
REPRESENTATION_ITEM('')
);
#143=(
BOUNDED_CURVE()
B_SPLINE_CURVE(2,(#34826,#34827,#34828,#34829,#34830,#34831,#34832,#34833,
#34834,#34835,#34836,#34837,#34838),.UNSPECIFIED.,.F.,.F.)
B_SPLINE_CURVE_WITH_KNOTS((3,2,2,2,2,2,3),(0.75,0.761904761904762,0.773809523809524,
0.785714285714286,0.797619047619048,0.809523809523809,0.821428571428572),
 .UNSPECIFIED.)
CURVE()
GEOMETRIC_REPRESENTATION_ITEM()
RATIONAL_B_SPLINE_CURVE((1.,0.866025403784439,1.,0.866025403784439,1.,0.866025403784439,
1.,0.866025403784439,1.,0.866025403784439,1.,0.866025403784439,1.))
REPRESENTATION_ITEM('')
);
#144=(
BOUNDED_CURVE()
B_SPLINE_CURVE(2,(#34843,#34844,#34845,#34846,#34847,#34848,#34849,#34850,
#34851,#34852,#34853,#34854,#34855),.UNSPECIFIED.,.F.,.F.)
B_SPLINE_CURVE_WITH_KNOTS((3,2,2,2,2,2,3),(0.678571428571429,0.690476190476191,
0.702380952380952,0.714285714285714,0.726190476190476,0.738095238095238,
0.75),.UNSPECIFIED.)
CURVE()
GEOMETRIC_REPRESENTATION_ITEM()
RATIONAL_B_SPLINE_CURVE((1.,0.866025403784439,1.,0.866025403784439,1.,0.866025403784439,
1.,0.866025403784439,1.,0.866025403784439,1.,0.866025403784439,1.))
REPRESENTATION_ITEM('')
);
#145=(
BOUNDED_CURVE()
B_SPLINE_CURVE(2,(#34856,#34857,#34858,#34859,#34860,#34861,#34862,#34863,
#34864,#34865,#34866,#34867,#34868),.UNSPECIFIED.,.F.,.F.)
B_SPLINE_CURVE_WITH_KNOTS((3,2,2,2,2,2,3),(0.678571428571429,0.690476190476191,
0.702380952380952,0.714285714285714,0.726190476190476,0.738095238095238,
0.75),.UNSPECIFIED.)
CURVE()
GEOMETRIC_REPRESENTATION_ITEM()
RATIONAL_B_SPLINE_CURVE((1.,0.866025403784439,1.,0.866025403784439,1.,0.866025403784439,
1.,0.866025403784439,1.,0.866025403784439,1.,0.866025403784439,1.))
REPRESENTATION_ITEM('')
);
#146=(
BOUNDED_CURVE()
B_SPLINE_CURVE(2,(#34873,#34874,#34875,#34876,#34877,#34878,#34879,#34880,
#34881,#34882,#34883,#34884,#34885),.UNSPECIFIED.,.F.,.F.)
B_SPLINE_CURVE_WITH_KNOTS((3,2,2,2,2,2,3),(0.607142857142857,0.619047619047619,
0.630952380952381,0.642857142857143,0.654761904761905,0.666666666666667,
0.678571428571429),.UNSPECIFIED.)
CURVE()
GEOMETRIC_REPRESENTATION_ITEM()
RATIONAL_B_SPLINE_CURVE((1.,0.866025403784439,1.,0.866025403784439,1.,0.866025403784439,
1.,0.866025403784439,1.,0.866025403784439,1.,0.866025403784439,1.))
REPRESENTATION_ITEM('')
);
#147=(
BOUNDED_CURVE()
B_SPLINE_CURVE(2,(#34886,#34887,#34888,#34889,#34890,#34891,#34892,#34893,
#34894,#34895,#34896,#34897,#34898),.UNSPECIFIED.,.F.,.F.)
B_SPLINE_CURVE_WITH_KNOTS((3,2,2,2,2,2,3),(0.607142857142857,0.619047619047619,
0.630952380952381,0.642857142857143,0.654761904761905,0.666666666666667,
0.678571428571429),.UNSPECIFIED.)
CURVE()
GEOMETRIC_REPRESENTATION_ITEM()
RATIONAL_B_SPLINE_CURVE((1.,0.866025403784439,1.,0.866025403784439,1.,0.866025403784439,
1.,0.866025403784439,1.,0.866025403784439,1.,0.866025403784439,1.))
REPRESENTATION_ITEM('')
);
#148=(
BOUNDED_CURVE()
B_SPLINE_CURVE(2,(#34903,#34904,#34905,#34906,#34907,#34908,#34909,#34910,
#34911,#34912,#34913,#34914,#34915),.UNSPECIFIED.,.F.,.F.)
B_SPLINE_CURVE_WITH_KNOTS((3,2,2,2,2,2,3),(0.535714285714286,0.547619047619048,
0.55952380952381,0.571428571428571,0.583333333333333,0.595238095238095,
0.607142857142857),.UNSPECIFIED.)
CURVE()
GEOMETRIC_REPRESENTATION_ITEM()
RATIONAL_B_SPLINE_CURVE((1.,0.866025403784439,1.,0.866025403784439,1.,0.866025403784439,
1.,0.866025403784439,1.,0.866025403784439,1.,0.866025403784439,1.))
REPRESENTATION_ITEM('')
);
#149=(
BOUNDED_CURVE()
B_SPLINE_CURVE(2,(#34916,#34917,#34918,#34919,#34920,#34921,#34922,#34923,
#34924,#34925,#34926,#34927,#34928),.UNSPECIFIED.,.F.,.F.)
B_SPLINE_CURVE_WITH_KNOTS((3,2,2,2,2,2,3),(0.535714285714286,0.547619047619048,
0.55952380952381,0.571428571428571,0.583333333333333,0.595238095238095,
0.607142857142857),.UNSPECIFIED.)
CURVE()
GEOMETRIC_REPRESENTATION_ITEM()
RATIONAL_B_SPLINE_CURVE((1.,0.866025403784439,1.,0.866025403784439,1.,0.866025403784439,
1.,0.866025403784439,1.,0.866025403784439,1.,0.866025403784439,1.))
REPRESENTATION_ITEM('')
);
#150=(
BOUNDED_CURVE()
B_SPLINE_CURVE(2,(#34933,#34934,#34935,#34936,#34937,#34938,#34939,#34940,
#34941,#34942,#34943,#34944,#34945),.UNSPECIFIED.,.F.,.F.)
B_SPLINE_CURVE_WITH_KNOTS((3,2,2,2,2,2,3),(0.464285714285714,0.476190476190476,
0.488095238095238,0.5,0.511904761904762,0.523809523809524,0.535714285714286),
 .UNSPECIFIED.)
CURVE()
GEOMETRIC_REPRESENTATION_ITEM()
RATIONAL_B_SPLINE_CURVE((1.,0.866025403784439,1.,0.866025403784439,1.,0.866025403784439,
1.,0.866025403784439,1.,0.866025403784439,1.,0.866025403784439,1.))
REPRESENTATION_ITEM('')
);
#151=(
BOUNDED_CURVE()
B_SPLINE_CURVE(2,(#34946,#34947,#34948,#34949,#34950,#34951,#34952,#34953,
#34954,#34955,#34956,#34957,#34958),.UNSPECIFIED.,.F.,.F.)
B_SPLINE_CURVE_WITH_KNOTS((3,2,2,2,2,2,3),(0.464285714285714,0.476190476190476,
0.488095238095238,0.5,0.511904761904762,0.523809523809524,0.535714285714286),
 .UNSPECIFIED.)
CURVE()
GEOMETRIC_REPRESENTATION_ITEM()
RATIONAL_B_SPLINE_CURVE((1.,0.866025403784439,1.,0.866025403784439,1.,0.866025403784439,
1.,0.866025403784439,1.,0.866025403784439,1.,0.866025403784439,1.))
REPRESENTATION_ITEM('')
);
#152=(
BOUNDED_CURVE()
B_SPLINE_CURVE(2,(#34963,#34964,#34965,#34966,#34967,#34968,#34969,#34970,
#34971,#34972,#34973,#34974,#34975),.UNSPECIFIED.,.F.,.F.)
B_SPLINE_CURVE_WITH_KNOTS((3,2,2,2,2,2,3),(0.392857142857143,0.404761904761905,
0.416666666666667,0.428571428571428,0.44047619047619,0.452380952380952,
0.464285714285714),.UNSPECIFIED.)
CURVE()
GEOMETRIC_REPRESENTATION_ITEM()
RATIONAL_B_SPLINE_CURVE((1.,0.866025403784439,1.,0.866025403784439,1.,0.866025403784439,
1.,0.866025403784439,1.,0.866025403784439,1.,0.866025403784439,1.))
REPRESENTATION_ITEM('')
);
#153=(
BOUNDED_CURVE()
B_SPLINE_CURVE(2,(#34976,#34977,#34978,#34979,#34980,#34981,#34982,#34983,
#34984,#34985,#34986,#34987,#34988),.UNSPECIFIED.,.F.,.F.)
B_SPLINE_CURVE_WITH_KNOTS((3,2,2,2,2,2,3),(0.392857142857143,0.404761904761905,
0.416666666666667,0.428571428571428,0.44047619047619,0.452380952380952,
0.464285714285714),.UNSPECIFIED.)
CURVE()
GEOMETRIC_REPRESENTATION_ITEM()
RATIONAL_B_SPLINE_CURVE((1.,0.866025403784439,1.,0.866025403784439,1.,0.866025403784439,
1.,0.866025403784439,1.,0.866025403784439,1.,0.866025403784439,1.))
REPRESENTATION_ITEM('')
);
#154=(
BOUNDED_CURVE()
B_SPLINE_CURVE(2,(#34993,#34994,#34995,#34996,#34997,#34998,#34999,#35000,
#35001,#35002,#35003,#35004,#35005),.UNSPECIFIED.,.F.,.F.)
B_SPLINE_CURVE_WITH_KNOTS((3,2,2,2,2,2,3),(0.321428571428572,0.333333333333334,
0.345238095238096,0.357142857142857,0.369047619047619,0.380952380952381,
0.392857142857143),.UNSPECIFIED.)
CURVE()
GEOMETRIC_REPRESENTATION_ITEM()
RATIONAL_B_SPLINE_CURVE((1.,0.866025403784439,1.,0.866025403784439,1.,0.866025403784439,
1.,0.866025403784439,1.,0.866025403784439,1.,0.866025403784439,1.))
REPRESENTATION_ITEM('')
);
#155=(
BOUNDED_CURVE()
B_SPLINE_CURVE(2,(#35006,#35007,#35008,#35009,#35010,#35011,#35012,#35013,
#35014,#35015,#35016,#35017,#35018),.UNSPECIFIED.,.F.,.F.)
B_SPLINE_CURVE_WITH_KNOTS((3,2,2,2,2,2,3),(0.321428571428572,0.333333333333334,
0.345238095238096,0.357142857142857,0.369047619047619,0.380952380952381,
0.392857142857143),.UNSPECIFIED.)
CURVE()
GEOMETRIC_REPRESENTATION_ITEM()
RATIONAL_B_SPLINE_CURVE((1.,0.866025403784439,1.,0.866025403784439,1.,0.866025403784439,
1.,0.866025403784439,1.,0.866025403784439,1.,0.866025403784439,1.))
REPRESENTATION_ITEM('')
);
#156=(
BOUNDED_CURVE()
B_SPLINE_CURVE(2,(#35023,#35024,#35025,#35026,#35027,#35028,#35029,#35030,
#35031,#35032,#35033,#35034,#35035),.UNSPECIFIED.,.F.,.F.)
B_SPLINE_CURVE_WITH_KNOTS((3,2,2,2,2,2,3),(0.25,0.261904761904762,0.273809523809524,
0.285714285714286,0.297619047619048,0.309523809523809,0.321428571428572),
 .UNSPECIFIED.)
CURVE()
GEOMETRIC_REPRESENTATION_ITEM()
RATIONAL_B_SPLINE_CURVE((1.,0.866025403784439,1.,0.866025403784439,1.,0.866025403784439,
1.,0.866025403784439,1.,0.866025403784439,1.,0.866025403784439,1.))
REPRESENTATION_ITEM('')
);
#157=(
BOUNDED_CURVE()
B_SPLINE_CURVE(2,(#35036,#35037,#35038,#35039,#35040,#35041,#35042,#35043,
#35044,#35045,#35046,#35047,#35048),.UNSPECIFIED.,.F.,.F.)
B_SPLINE_CURVE_WITH_KNOTS((3,2,2,2,2,2,3),(0.25,0.261904761904762,0.273809523809524,
0.285714285714286,0.297619047619048,0.309523809523809,0.321428571428572),
 .UNSPECIFIED.)
CURVE()
GEOMETRIC_REPRESENTATION_ITEM()
RATIONAL_B_SPLINE_CURVE((1.,0.866025403784439,1.,0.866025403784439,1.,0.866025403784439,
1.,0.866025403784439,1.,0.866025403784439,1.,0.866025403784439,1.))
REPRESENTATION_ITEM('')
);
#158=(
BOUNDED_CURVE()
B_SPLINE_CURVE(2,(#35053,#35054,#35055,#35056,#35057,#35058,#35059,#35060,
#35061,#35062,#35063,#35064,#35065),.UNSPECIFIED.,.F.,.F.)
B_SPLINE_CURVE_WITH_KNOTS((3,2,2,2,2,2,3),(0.178571428571428,0.19047619047619,
0.202380952380952,0.214285714285714,0.226190476190476,0.238095238095238,
0.25),.UNSPECIFIED.)
CURVE()
GEOMETRIC_REPRESENTATION_ITEM()
RATIONAL_B_SPLINE_CURVE((1.,0.866025403784439,1.,0.866025403784439,1.,0.866025403784439,
1.,0.866025403784439,1.,0.866025403784439,1.,0.866025403784439,1.))
REPRESENTATION_ITEM('')
);
#159=(
BOUNDED_CURVE()
B_SPLINE_CURVE(2,(#35066,#35067,#35068,#35069,#35070,#35071,#35072,#35073,
#35074,#35075,#35076,#35077,#35078),.UNSPECIFIED.,.F.,.F.)
B_SPLINE_CURVE_WITH_KNOTS((3,2,2,2,2,2,3),(0.178571428571428,0.19047619047619,
0.202380952380952,0.214285714285714,0.226190476190476,0.238095238095238,
0.25),.UNSPECIFIED.)
CURVE()
GEOMETRIC_REPRESENTATION_ITEM()
RATIONAL_B_SPLINE_CURVE((1.,0.866025403784439,1.,0.866025403784439,1.,0.866025403784439,
1.,0.866025403784439,1.,0.866025403784439,1.,0.866025403784439,1.))
REPRESENTATION_ITEM('')
);
#160=(
BOUNDED_CURVE()
B_SPLINE_CURVE(2,(#35083,#35084,#35085,#35086,#35087,#35088,#35089,#35090,
#35091,#35092,#35093,#35094,#35095),.UNSPECIFIED.,.F.,.F.)
B_SPLINE_CURVE_WITH_KNOTS((3,2,2,2,2,2,3),(0.107142857142857,0.119047619047619,
0.130952380952381,0.142857142857143,0.154761904761905,0.166666666666667,
0.178571428571428),.UNSPECIFIED.)
CURVE()
GEOMETRIC_REPRESENTATION_ITEM()
RATIONAL_B_SPLINE_CURVE((1.,0.866025403784439,1.,0.866025403784439,1.,0.866025403784439,
1.,0.866025403784439,1.,0.866025403784439,1.,0.866025403784439,1.))
REPRESENTATION_ITEM('')
);
#161=(
BOUNDED_CURVE()
B_SPLINE_CURVE(2,(#35096,#35097,#35098,#35099,#35100,#35101,#35102,#35103,
#35104,#35105,#35106,#35107,#35108),.UNSPECIFIED.,.F.,.F.)
B_SPLINE_CURVE_WITH_KNOTS((3,2,2,2,2,2,3),(0.107142857142857,0.119047619047619,
0.130952380952381,0.142857142857143,0.154761904761905,0.166666666666667,
0.178571428571428),.UNSPECIFIED.)
CURVE()
GEOMETRIC_REPRESENTATION_ITEM()
RATIONAL_B_SPLINE_CURVE((1.,0.866025403784439,1.,0.866025403784439,1.,0.866025403784439,
1.,0.866025403784439,1.,0.866025403784439,1.,0.866025403784439,1.))
REPRESENTATION_ITEM('')
);
#162=(
BOUNDED_CURVE()
B_SPLINE_CURVE(2,(#35114,#35115,#35116,#35117,#35118,#35119,#35120),
 .UNSPECIFIED.,.F.,.F.)
B_SPLINE_CURVE_WITH_KNOTS((3,2,2,3),(0.,0.0119047619047619,0.0238095238095238,
0.0357142857142857),.UNSPECIFIED.)
CURVE()
GEOMETRIC_REPRESENTATION_ITEM()
RATIONAL_B_SPLINE_CURVE((1.,0.866025403784439,1.,0.866025403784439,1.,0.866025403784439,
1.))
REPRESENTATION_ITEM('')
);
#163=(
BOUNDED_CURVE()
B_SPLINE_CURVE(2,(#35123,#35124,#35125,#35126,#35127,#35128,#35129),
 .UNSPECIFIED.,.F.,.F.)
B_SPLINE_CURVE_WITH_KNOTS((3,2,2,3),(0.,0.0119047619047619,0.0238095238095238,
0.0357142857142857),.UNSPECIFIED.)
CURVE()
GEOMETRIC_REPRESENTATION_ITEM()
RATIONAL_B_SPLINE_CURVE((1.,0.866025403784439,1.,0.866025403784439,1.,0.866025403784439,
1.))
REPRESENTATION_ITEM('')
);
#164=(
BOUNDED_CURVE()
B_SPLINE_CURVE(2,(#35193,#35194,#35195,#35196,#35197,#35198,#35199,#35200,
#35201,#35202,#35203,#35204,#35205),.UNSPECIFIED.,.F.,.F.)
B_SPLINE_CURVE_WITH_KNOTS((3,2,2,2,2,2,3),(0.,0.0119047619047619,0.0238095238095238,
0.0357142857142857,0.0476190476190476,0.0595238095238095,0.0626545676342116),
 .UNSPECIFIED.)
CURVE()
GEOMETRIC_REPRESENTATION_ITEM()
RATIONAL_B_SPLINE_CURVE((1.,0.866025403784439,1.,0.866025403784439,1.,0.866025403784439,
1.,0.866025403784439,1.,0.866025403784439,1.,0.964766867490064,0.948065212760667))
REPRESENTATION_ITEM('')
);
#165=(
BOUNDED_CURVE()
B_SPLINE_CURVE(2,(#35549,#35550,#35551,#35552,#35553,#35554,#35555,#35556,
#35557,#35558,#35559,#35560,#35561),.UNSPECIFIED.,.F.,.F.)
B_SPLINE_CURVE_WITH_KNOTS((3,2,2,2,2,2,3),(0.0357142857142857,0.0476190476190476,
0.0595238095238095,0.0714285714285714,0.0833333333333333,0.0952380952380952,
0.107142857142857),.UNSPECIFIED.)
CURVE()
GEOMETRIC_REPRESENTATION_ITEM()
RATIONAL_B_SPLINE_CURVE((1.,0.866025403784439,1.,0.866025403784439,1.,0.866025403784439,
1.,0.866025403784439,1.,0.866025403784439,1.,0.866025403784439,1.))
REPRESENTATION_ITEM('')
);
#166=(
BOUNDED_CURVE()
B_SPLINE_CURVE(2,(#35600,#35601,#35602,#35603,#35604,#35605,#35606,#35607,
#35608,#35609,#35610,#35611,#35612),.UNSPECIFIED.,.F.,.F.)
B_SPLINE_CURVE_WITH_KNOTS((3,2,2,2,2,2,3),(0.0357142857142857,0.0476190476190476,
0.0595238095238095,0.0714285714285714,0.0833333333333333,0.0952380952380952,
0.107142857142857),.UNSPECIFIED.)
CURVE()
GEOMETRIC_REPRESENTATION_ITEM()
RATIONAL_B_SPLINE_CURVE((1.,0.866025403784439,1.,0.866025403784439,1.,0.866025403784439,
1.,0.866025403784439,1.,0.866025403784439,1.,0.866025403784439,1.))
REPRESENTATION_ITEM('')
);
#167=(
BOUNDED_CURVE()
B_SPLINE_CURVE(2,(#35989,#35990,#35991,#35992,#35993,#35994,#35995),
 .UNSPECIFIED.,.F.,.F.)
B_SPLINE_CURVE_WITH_KNOTS((3,2,2,3),(0.96944370253851,0.976190476190476,
0.988095238095238,1.),.UNSPECIFIED.)
CURVE()
GEOMETRIC_REPRESENTATION_ITEM()
RATIONAL_B_SPLINE_CURVE((0.934205814715249,0.924072712834481,1.,0.866025403784439,
1.,0.866025403784439,1.))
REPRESENTATION_ITEM('')
);
#168=CONICAL_SURFACE('',#18363,17.5,0.0444152152469099);
#169=CONICAL_SURFACE('',#18378,31.5,1.55500816505907);
#170=CONICAL_SURFACE('',#18555,17.5,0.038076825589802);
#171=CONICAL_SURFACE('',#18583,1.6,0.785398163397458);
#172=CONICAL_SURFACE('',#18587,1.6,0.785398163397457);
#173=CONICAL_SURFACE('',#18591,1.6,0.785398163397458);
#174=CONICAL_SURFACE('',#18595,1.6,0.785398163397457);
#175=CONICAL_SURFACE('',#18599,1.6,0.785398163397457);
#176=CONICAL_SURFACE('',#18603,1.6,0.785398163397457);
#177=CONICAL_SURFACE('',#18607,1.6,0.785398163397457);
#178=CONICAL_SURFACE('',#18611,1.6,0.785398163397457);
#179=CONICAL_SURFACE('',#18615,1.6,0.785398163397457);
#180=CONICAL_SURFACE('',#18619,2.1,0.785398163397457);
#181=CONICAL_SURFACE('',#18623,1.6,0.785398163397458);
#182=CONICAL_SURFACE('',#18627,1.6,0.785398163397458);
#183=CONICAL_SURFACE('',#18631,1.6,0.785398163397457);
#184=CONICAL_SURFACE('',#18888,14.,0.908165646210649);
#185=CONICAL_SURFACE('',#19072,1.60000000000001,0.785398163397451);
#186=CONICAL_SURFACE('',#19074,2.,0.785398163397449);
#187=CONICAL_SURFACE('',#19076,3.99999999999999,0.785398163397452);
#188=CONICAL_SURFACE('',#19078,3.6,0.785398163397448);
#189=CONICAL_SURFACE('',#19172,4.,0.785398163397449);
#190=CONICAL_SURFACE('',#19250,1.6,0.78539816339745);
#191=CONICAL_SURFACE('',#19252,2.,0.785398163397445);
#192=CONICAL_SURFACE('',#19253,3.6,0.785398163397445);
#193=TOROIDAL_SURFACE('',#18311,15.5,0.3);
#194=TOROIDAL_SURFACE('',#18315,31.2,0.3);
#195=TOROIDAL_SURFACE('',#18320,12.8,0.3);
#196=TOROIDAL_SURFACE('',#18325,10.5,0.3);
#197=TOROIDAL_SURFACE('',#18329,10.5,0.3);
#198=TOROIDAL_SURFACE('',#18334,31.2,0.3);
#199=TOROIDAL_SURFACE('',#18338,18.2,0.3);
#200=TOROIDAL_SURFACE('',#18342,17.2130371832119,0.3);
#201=TOROIDAL_SURFACE('',#18346,16.1,0.3);
#202=TOROIDAL_SURFACE('',#18380,31.25,0.25);
#203=TOROIDAL_SURFACE('',#18385,19.75,0.25);
#204=TOROIDAL_SURFACE('',#18389,17.75,0.25);
#205=TOROIDAL_SURFACE('',#18399,18.1406575306034,0.25);
#206=TOROIDAL_SURFACE('',#18405,19.25,0.25);
#207=TOROIDAL_SURFACE('',#18411,17.759705149651,0.25);
#208=TOROIDAL_SURFACE('',#18414,19.25,0.25);
#209=TOROIDAL_SURFACE('',#18425,17.759705149651,0.25);
#210=TOROIDAL_SURFACE('',#18431,19.25,0.25);
#211=TOROIDAL_SURFACE('',#18435,18.1406575306034,0.25);
#212=TOROIDAL_SURFACE('',#18439,19.25,0.25);
#213=TOROIDAL_SURFACE('',#18452,18.1406575306034,0.25);
#214=TOROIDAL_SURFACE('',#18458,19.25,0.25);
#215=TOROIDAL_SURFACE('',#18462,17.759705149651,0.25);
#216=TOROIDAL_SURFACE('',#18465,19.25,0.25);
#217=TOROIDAL_SURFACE('',#18479,17.759705149651,0.25);
#218=TOROIDAL_SURFACE('',#18485,19.25,0.25);
#219=TOROIDAL_SURFACE('',#18490,18.1406575306034,0.25);
#220=TOROIDAL_SURFACE('',#18493,19.25,0.25);
#221=TOROIDAL_SURFACE('',#18506,18.1406575306034,0.25);
#222=TOROIDAL_SURFACE('',#18513,19.25,0.25);
#223=TOROIDAL_SURFACE('',#18520,17.759705149651,0.25);
#224=TOROIDAL_SURFACE('',#18523,19.25,0.25);
#225=TOROIDAL_SURFACE('',#18530,31.25,0.25);
#226=TOROIDAL_SURFACE('',#18551,18.2999999294072,0.8);
#227=TOROIDAL_SURFACE('',#18885,9.1242968857267,4.22441061393973);
#228=TOROIDAL_SURFACE('',#18911,6.3,0.3);
#229=TOROIDAL_SURFACE('',#18913,9.7,0.3);
#230=TOROIDAL_SURFACE('',#19215,11.8,0.2);
#231=TOROIDAL_SURFACE('',#19220,11.8,0.2);
#232=TOROIDAL_SURFACE('',#19225,3.45,0.2);
#233=TOROIDAL_SURFACE('',#19230,3.45,0.2);
#234=TOROIDAL_SURFACE('',#19260,4.5,0.5);
#235=TOROIDAL_SURFACE('',#19264,4.5,0.5);
#236=B_SPLINE_CURVE_WITH_KNOTS('',3,(#25581,#25582,#25583,#25584,#25585,
#25586,#25587,#25588,#25589,#25590,#25591,#25592),.UNSPECIFIED.,.F.,.F.,
(4,2,2,2,2,4),(-0.0307505677232343,-0.0290851658458097,-0.0274197639683852,
-0.0256899175968281,-0.0239600712252709,-0.0214016072500974),
 .UNSPECIFIED.);
#237=B_SPLINE_CURVE_WITH_KNOTS('',3,(#25608,#25609,#25610,#25611,#25612,
#25613,#25614,#25615,#25616,#25617,#25618,#25619),.UNSPECIFIED.,.F.,.F.,
(4,2,2,2,2,4),(-0.0400996909613273,-0.0375410642212333,-0.035811217849675,
-0.0340813714781167,-0.0324159696006892,-0.0307505677232617),
 .UNSPECIFIED.);
#238=B_SPLINE_CURVE_WITH_KNOTS('',3,(#25634,#25635,#25636,#25637,#25638,
#25639,#25640,#25641,#25642,#25643,#25644,#25645),.UNSPECIFIED.,.F.,.F.,
(4,2,2,2,2,4),(0.0307505677231893,0.0324159696006138,0.0340813714780383,
0.0358112178495909,0.0375410642211435,0.040099528194227),.UNSPECIFIED.);
#239=B_SPLINE_CURVE_WITH_KNOTS('',3,(#25652,#25653,#25654,#25655,#25656,
#25657,#25658,#25659,#25660,#25661,#25662,#25663),.UNSPECIFIED.,.F.,.F.,
(4,2,2,2,2,4),(0.0214015561623852,0.0239600712252435,0.0256899175967988,
0.0274197639683542,0.0290851658457769,0.0307505677231996),.UNSPECIFIED.);
#240=B_SPLINE_CURVE_WITH_KNOTS('',3,(#25749,#25750,#25751,#25752,#25753,
#25754,#25755,#25756,#25757,#25758,#25759,#25760),.UNSPECIFIED.,.F.,.F.,
(4,2,2,2,2,4),(0.0214014871422872,0.0239600712252674,0.0256899175968258,
0.0274197639683841,0.0290851658458094,0.0307505677232346),.UNSPECIFIED.);
#241=B_SPLINE_CURVE_WITH_KNOTS('',3,(#25762,#25763,#25764,#25765,#25766,
#25767),.UNSPECIFIED.,.F.,.F.,(4,2,4),(0.516167584835576,0.556355629697994,
0.571945746029783),.UNSPECIFIED.);
#242=B_SPLINE_CURVE_WITH_KNOTS('',3,(#25770,#25771,#25772,#25773,#25774,
#25775),.UNSPECIFIED.,.F.,.F.,(4,2,4),(-0.572283818814118,-0.556572033620994,
-0.516504886359884),.UNSPECIFIED.);
#243=B_SPLINE_CURVE_WITH_KNOTS('',3,(#25778,#25779,#25780,#25781,#25782,
#25783),.UNSPECIFIED.,.F.,.F.,(4,2,4),(0.516062927236787,0.556286483365537,
0.571840801367595),.UNSPECIFIED.);
#244=B_SPLINE_CURVE_WITH_KNOTS('',3,(#25787,#25788,#25789,#25790,#25791,
#25792),.UNSPECIFIED.,.F.,.F.,(4,2,4),(-0.572388774164482,-0.556641170070289,
-0.516609564275015),.UNSPECIFIED.);
#245=B_SPLINE_CURVE_WITH_KNOTS('',3,(#25794,#25795,#25796,#25797,#25798,
#25799,#25800,#25801,#25802,#25803,#25804,#25805),.UNSPECIFIED.,.F.,.F.,
(4,2,2,2,2,4),(0.0307505677232594,0.0324159696006859,0.0340813714781124,
0.0358112178496696,0.0375410642212269,0.0400994853939697),.UNSPECIFIED.);
#246=B_SPLINE_CURVE_WITH_KNOTS('',3,(#25809,#25810,#25811,#25812,#25813,
#25814,#25815,#25816,#25817,#25818,#25819,#25820),.UNSPECIFIED.,.F.,.F.,
(4,2,2,2,2,4),(0.0214014871425106,0.0239600712253013,0.0256899175968606,
0.0274197639684198,0.0290851658458467,0.0307505677232736),.UNSPECIFIED.);
#247=B_SPLINE_CURVE_WITH_KNOTS('',3,(#25822,#25823,#25824,#25825,#25826,
#25827),.UNSPECIFIED.,.F.,.F.,(4,2,4),(0.516167584819259,0.556355629663768,
0.571945746013171),.UNSPECIFIED.);
#248=B_SPLINE_CURVE_WITH_KNOTS('',3,(#25830,#25831,#25832,#25833,#25834,
#25835),.UNSPECIFIED.,.F.,.F.,(4,2,4),(-0.572283818796558,-0.556572033600684,
-0.516504886344356),.UNSPECIFIED.);
#249=B_SPLINE_CURVE_WITH_KNOTS('',3,(#25839,#25840,#25841,#25842,#25843,
#25844,#25845,#25846,#25847,#25848,#25849,#25850),.UNSPECIFIED.,.F.,.F.,
(4,2,2,2,2,4),(0.0214015561620376,0.0239600712252775,0.0256899175968367,
0.0274197639683959,0.0290851658458218,0.0307505677232477),.UNSPECIFIED.);
#250=B_SPLINE_CURVE_WITH_KNOTS('',3,(#25852,#25853,#25854,#25855,#25856,
#25857),.UNSPECIFIED.,.F.,.F.,(4,2,4),(0.516336929306378,0.556467476401172,
0.572115549692269),.UNSPECIFIED.);
#251=B_SPLINE_CURVE_WITH_KNOTS('',3,(#25861,#25862,#25863,#25864,#25865,
#25866),.UNSPECIFIED.,.F.,.F.,(4,2,4),(-0.572113997134204,-0.556460133617456,
-0.516335518817303),.UNSPECIFIED.);
#252=B_SPLINE_CURVE_WITH_KNOTS('',3,(#25868,#25869,#25870,#25871,#25872,
#25873,#25874,#25875,#25876,#25877,#25878,#25879),.UNSPECIFIED.,.F.,.F.,
(4,2,2,2,2,4),(0.0307505677232669,0.0324159696006922,0.0340813714781176,
0.0358112178496757,0.0375410642212338,0.0400995974505249),.UNSPECIFIED.);
#253=B_SPLINE_CURVE_WITH_KNOTS('',3,(#25882,#25883,#25884,#25885,#25886,
#25887),.UNSPECIFIED.,.F.,.F.,(4,2,4),(0.516336929316142,0.556467476363535,
0.572115549701707),.UNSPECIFIED.);
#254=B_SPLINE_CURVE_WITH_KNOTS('',3,(#25891,#25892,#25893,#25894,#25895,
#25896),.UNSPECIFIED.,.F.,.F.,(4,2,4),(-0.572087843455165,-0.556460133653863,
-0.516335518814487),.UNSPECIFIED.);
#255=B_SPLINE_CURVE_WITH_KNOTS('',3,(#25898,#25899,#25900,#25901,#25902,
#25903,#25904,#25905,#25906,#25907,#25908,#25909),.UNSPECIFIED.,.F.,.F.,
(4,2,2,2,2,4),(0.0307505677231587,0.0324159696005802,0.0340813714780017,
0.0358112178495531,0.0375410642211044,0.0401277329731923),.UNSPECIFIED.);
#256=B_SPLINE_CURVE_WITH_KNOTS('',3,(#25915,#25916,#25917,#25918,#25919,
#25920,#25921,#25922,#25923,#25924,#25925,#25926,#25927,#25928,#25929,#25930,
#25931,#25932,#25933,#25934,#25935,#25936),.UNSPECIFIED.,.F.,.F.,(4,2,2,
2,2,2,2,2,2,2,4),(2.02457825278125E-10,0.00248408483075073,0.00372612724612612,
0.00434714845381382,0.00465765905765771,0.00481291435957969,0.00489054201054069,
0.00492935583602118,0.00494876274876143,0.00495846620513155,0.00496816966150168),
 .UNSPECIFIED.);
#257=B_SPLINE_CURVE_WITH_KNOTS('',3,(#25938,#25939,#25940,#25941,#25942,
#25943,#25944,#25945,#25946,#25947,#25948,#25949,#25950,#25951,#25952,#25953,
#25954,#25955,#25956,#25957,#25958,#25959),.UNSPECIFIED.,.F.,.F.,(4,2,2,
2,2,2,2,2,2,2,4),(3.5048712953905E-5,4.4761383731225E-5,5.4474054508545E-5,
7.38993960631036E-5,0.00011275007917231,0.000190451445390804,0.000345854177827798,
0.000656659642701783,0.00127827057244967,0.00252149243194545,0.00500793615093709),
 .UNSPECIFIED.);
#258=B_SPLINE_CURVE_WITH_KNOTS('',3,(#25962,#25963,#25964,#25965,#25966,
#25967,#25968,#25969,#25970,#25971,#25972,#25973,#25974,#25975,#25976,#25977,
#25978,#25979,#25980,#25981,#25982,#25983),.UNSPECIFIED.,.F.,.F.,(4,2,2,
2,2,2,2,2,2,2,4),(2.04137276529534E-10,0.00248408522863344,0.00372612784295016,
0.00434714915010856,0.00465765980368776,0.00481291513047741,0.00489054279387223,
0.00492935662556968,0.00494876354141844,0.00495846699934282,0.0049681704572672),
 .UNSPECIFIED.);
#259=B_SPLINE_CURVE_WITH_KNOTS('',3,(#25985,#25986,#25987,#25988,#25989,
#25990,#25991,#25992,#25993,#25994,#25995,#25996,#25997,#25998,#25999,#26000,
#26001,#26002,#26003,#26004,#26005,#26006),.UNSPECIFIED.,.F.,.F.,(4,2,2,
2,2,2,2,2,2,2,4),(3.50520341719619E-5,4.47649965919165E-5,5.44779590118712E-5,
7.3903883851858E-5,0.000112755733531832,0.0001904594328917,0.000345866831611521,
0.000656681629051249,0.00127831122393071,0.00252157041368962,0.00500808879320745),
 .UNSPECIFIED.);
#260=B_SPLINE_CURVE_WITH_KNOTS('',3,(#26014,#26015,#26016,#26017,#26018,
#26019,#26020,#26021,#26022,#26023,#26024,#26025,#26026,#26027,#26028,#26029,
#26030,#26031,#26032,#26033,#26034,#26035),.UNSPECIFIED.,.F.,.F.,(4,2,2,
2,2,2,2,2,2,2,4),(2.06866606511861E-10,0.00248408587267595,0.00372612880901388,
0.00434715027718289,0.00465766101126744,0.00481291637830975,0.00489054406183091,
0.00492935790359148,0.00494876482447177,0.00495846828491192,0.00496817174535206),
 .UNSPECIFIED.);
#261=B_SPLINE_CURVE_WITH_KNOTS('',3,(#26037,#26038,#26039,#26040,#26041,
#26042,#26043,#26044,#26045,#26046,#26047,#26048,#26049,#26050,#26051,#26052,
#26053,#26054,#26055,#26056,#26057,#26058),.UNSPECIFIED.,.F.,.F.,(4,2,2,
2,2,2,2,2,2,2,4),(3.50574081053878E-5,4.47708507809905E-5,5.44842934565933E-5,
7.39111788077861E-5,0.000112764949510167,0.000190472490915007,0.000345887573724691,
0.000656717739344059,0.00127837807058271,0.00252169873306001,0.00500834005801461),
 .UNSPECIFIED.);
#262=B_SPLINE_CURVE_WITH_KNOTS('',3,(#26061,#26062,#26063,#26064,#26065,
#26066,#26067,#26068,#26069,#26070,#26071,#26072,#26073,#26074,#26075,#26076,
#26077,#26078,#26079,#26080,#26081,#26082),.UNSPECIFIED.,.F.,.F.,(4,2,2,
2,2,2,2,2,2,2,4),(2.06867445612259E-10,0.00248408587267104,0.00372612880900657,
0.00434715027717433,0.00465766101125817,0.00481291637830013,0.00489054406182111,
0.0049293579035816,0.00494876482446188,0.00495846828490199,0.00496817174534209),
 .UNSPECIFIED.);
#263=B_SPLINE_CURVE_WITH_KNOTS('',3,(#26084,#26085,#26086,#26087,#26088,
#26089,#26090,#26091,#26092,#26093,#26094,#26095,#26096,#26097,#26098,#26099,
#26100,#26101,#26102,#26103,#26104,#26105),.UNSPECIFIED.,.F.,.F.,(4,2,2,
2,2,2,2,2,2,2,4),(3.50574081266199E-5,4.47708505998206E-5,5.44842930730214E-5,
7.39111780194308E-5,0.000112764947912246,0.000190472487697963,0.000345887567269397,
0.000656717726412263,0.001278378044698,0.00252169868126955,0.00500833995441257),
 .UNSPECIFIED.);
#264=B_SPLINE_CURVE_WITH_KNOTS('',3,(#26108,#26109,#26110,#26111,#26112,
#26113,#26114,#26115,#26116,#26117,#26118,#26119,#26120,#26121,#26122,#26123,
#26124,#26125,#26126,#26127,#26128,#26129),.UNSPECIFIED.,.F.,.F.,(4,2,2,
2,2,2,2,2,2,2,4),(2.04137059199594E-10,0.00248408522863389,0.00372612784295087,
0.00434714915010935,0.00465765980368859,0.00481291513047817,0.00489054279387297,
0.00492935662557032,0.00494876354141895,0.00495846699934332,0.00496817045726768),
 .UNSPECIFIED.);
#265=B_SPLINE_CURVE_WITH_KNOTS('',3,(#26130,#26131,#26132,#26133,#26134,
#26135,#26136,#26137,#26138,#26139,#26140,#26141,#26142,#26143,#26144,#26145,
#26146,#26147,#26148,#26149,#26150,#26151),.UNSPECIFIED.,.F.,.F.,(4,2,2,
2,2,2,2,2,2,2,4),(3.50520341720812E-5,4.47649965026772E-5,5.44779588332732E-5,
7.39038834943838E-5,0.000112755732816681,0.00019045943146128,0.000345866828750562,
0.00065668162332904,0.00127831121248599,0.00252157039079989,0.00500808874742778),
 .UNSPECIFIED.);
#266=B_SPLINE_CURVE_WITH_KNOTS('',3,(#26205,#26206,#26207,#26208,#26209,
#26210,#26211,#26212,#26213,#26214,#26215,#26216,#26217,#26218),
 .UNSPECIFIED.,.F.,.F.,(4,2,2,2,2,2,4),(-0.000304965314045538,0.,0.000936499595052828,
0.00576011793928687,0.00947606916598535,0.0122802204486003,0.0139854910646116),
 .UNSPECIFIED.);
#267=B_SPLINE_CURVE_WITH_KNOTS('',3,(#26225,#26226,#26227,#26228,#26229,
#26230,#26231,#26232,#26233,#26234,#26235,#26236,#26237,#26238,#26239,#26240),
 .UNSPECIFIED.,.F.,.F.,(4,2,2,2,2,2,2,4),(0.0536858997421767,0.0538805473387552,
0.0625727109542441,0.0725640535967514,0.0859159770081403,0.0987536985065928,
0.112218387900172,0.112607088674662),.UNSPECIFIED.);
#268=B_SPLINE_CURVE_WITH_KNOTS('',3,(#26255,#26256,#26257,#26258,#26259,
#26260,#26261,#26262,#26263,#26264,#26265,#26266,#26267,#26268,#26269,#26270),
 .UNSPECIFIED.,.F.,.F.,(4,2,2,2,2,2,2,4),(-0.0122740412193648,-0.0121759293582432,
-0.0120897396500415,-0.0111319415843575,-0.00947389246986148,-0.00820108783558479,
-0.0071868786468098,-0.00688693855294442),.UNSPECIFIED.);
#269=B_SPLINE_CURVE_WITH_KNOTS('',3,(#26276,#26277,#26278,#26279,#26280,
#26281,#26282,#26283,#26284,#26285,#26286,#26287,#26288,#26289,#26290,#26291),
 .UNSPECIFIED.,.F.,.F.,(4,2,2,2,2,2,2,4),(-0.0477691295327812,-0.0476102750821729,
-0.0405164866112679,-0.0323624211355981,-0.0214657417184032,-0.0109887092110674,
0.,0.000317223788085325),.UNSPECIFIED.);
#270=B_SPLINE_CURVE_WITH_KNOTS('',3,(#26303,#26304,#26305,#26306,#26307,
#26308,#26309,#26310,#26311,#26312,#26313,#26314,#26315,#26316,#26317,#26318),
 .UNSPECIFIED.,.F.,.F.,(4,2,2,2,2,2,2,4),(0.00685142344086609,0.00716754606670829,
0.00817883021840179,0.00945159950065682,0.0111102560598908,0.0126000677878647,
0.0134555802450022,0.0143116650403246),.UNSPECIFIED.);
#271=B_SPLINE_CURVE_WITH_KNOTS('',3,(#26340,#26341,#26342,#26343,#26344,
#26345,#26346,#26347,#26348,#26349,#26350,#26351,#26352,#26353,#26354,#26355),
 .UNSPECIFIED.,.F.,.F.,(4,2,2,2,2,2,2,4),(-0.000317223787690337,3.02215934569472E-15,
0.0109887092111399,0.0214657417185508,0.0323624211357588,0.0405164866114483,
0.0476102750823548,0.047769129532989),.UNSPECIFIED.);
#272=B_SPLINE_CURVE_WITH_KNOTS('',3,(#26359,#26360,#26361,#26362,#26363,
#26364,#26365,#26366,#26367,#26368,#26369,#26370,#26371,#26372),
 .UNSPECIFIED.,.F.,.F.,(4,2,2,2,2,2,4),(-0.0138875980614929,-0.0121989286884961,
-0.00941634599982081,-0.00572975137256096,-0.00094390537822651,0.,0.000305060128611046),
 .UNSPECIFIED.);
#273=B_SPLINE_CURVE_WITH_KNOTS('',3,(#26384,#26385,#26386,#26387,#26388,
#26389,#26390,#26391,#26392,#26393,#26394,#26395,#26396,#26397,#26398,#26399),
 .UNSPECIFIED.,.F.,.F.,(4,2,2,2,2,2,2,4),(-0.112607088625168,-0.112218387851368,
-0.0987536984648267,-0.0859159769729998,-0.0725640535676872,-0.0625727109298437,
-0.0538805473185267,-0.053685899721448),.UNSPECIFIED.);
#274=B_SPLINE_CURVE_WITH_KNOTS('',3,(#26440,#26441,#26442,#26443,#26444,
#26445,#26446,#26447,#26448,#26449,#26450,#26451,#26452,#26453),
 .UNSPECIFIED.,.F.,.F.,(4,2,2,2,2,2,4),(-0.000304965268692175,0.,0.000936496117482782,
0.00576013224595397,0.00947609729856078,0.0122802587445126,0.0139855371807907),
 .UNSPECIFIED.);
#275=B_SPLINE_CURVE_WITH_KNOTS('',3,(#26463,#26464,#26465,#26466,#26467,
#26468,#26469,#26470,#26471,#26472,#26473,#26474,#26475,#26476,#26477,#26478),
 .UNSPECIFIED.,.F.,.F.,(4,2,2,2,2,2,2,4),(0.0536858997392164,0.0538805473358447,
0.0625727109506776,0.072564053592395,0.0859159770028611,0.0987536985002761,
0.112218387892815,0.112607088666955),.UNSPECIFIED.);
#276=B_SPLINE_CURVE_WITH_KNOTS('',3,(#26492,#26493,#26494,#26495,#26496,
#26497,#26498,#26499,#26500,#26501,#26502,#26503,#26504,#26505,#26506,#26507),
 .UNSPECIFIED.,.F.,.F.,(4,2,2,2,2,2,2,4),(-0.0122740769336355,-0.0121759644410632,
-0.0120897737524462,-0.0111319575392944,-0.00947390765146132,-0.00820110219546828,
-0.00718689112173828,-0.00688695772759274),.UNSPECIFIED.);
#277=B_SPLINE_CURVE_WITH_KNOTS('',3,(#26513,#26514,#26515,#26516,#26517,
#26518,#26519,#26520,#26521,#26522,#26523,#26524,#26525,#26526,#26527,#26528),
 .UNSPECIFIED.,.F.,.F.,(4,2,2,2,2,2,2,4),(-0.0477691295328705,-0.0476102750818484,
-0.0405164866108641,-0.0323624211350328,-0.0214657417175428,-0.0109887092105592,
0.,0.00031722378862325),.UNSPECIFIED.);
#278=B_SPLINE_CURVE_WITH_KNOTS('',3,(#26544,#26545,#26546,#26547,#26548,
#26549,#26550,#26551,#26552,#26553,#26554,#26555,#26556,#26557,#26558,#26559),
 .UNSPECIFIED.,.F.,.F.,(4,2,2,2,2,2,2,4),(0.00683098498387795,0.00715685727468737,
0.0081665770863791,0.0094395668715797,0.0110988523787266,0.0125271081563038,
0.0131709865966103,0.0138210554549785),.UNSPECIFIED.);
#279=B_SPLINE_CURVE_WITH_KNOTS('',3,(#26580,#26581,#26582,#26583,#26584,
#26585,#26586,#26587,#26588,#26589,#26590,#26591,#26592,#26593,#26594,#26595),
 .UNSPECIFIED.,.F.,.F.,(4,2,2,2,2,2,2,4),(-0.000317223788318669,0.,0.0109887092111283,
0.0214657417185403,0.0323624211358337,0.0405164866115566,0.0476102750824874,
0.0477691295331555),.UNSPECIFIED.);
#280=B_SPLINE_CURVE_WITH_KNOTS('',3,(#26599,#26600,#26601,#26602,#26603,
#26604,#26605,#26606,#26607,#26608,#26609,#26610,#26611,#26612),
 .UNSPECIFIED.,.F.,.F.,(4,2,2,2,2,2,4),(-0.013826978099047,-0.0121485991715528,
-0.00937937937785604,-0.00571097373361621,-0.000948519651099016,0.,0.00030511843446065),
 .UNSPECIFIED.);
#281=B_SPLINE_CURVE_WITH_KNOTS('',3,(#26624,#26625,#26626,#26627,#26628,
#26629,#26630,#26631,#26632,#26633,#26634,#26635,#26636,#26637,#26638,#26639),
 .UNSPECIFIED.,.F.,.F.,(4,2,2,2,2,2,2,4),(-0.112607088663875,-0.112218387889847,
-0.0987536984976824,-0.0859159770006442,-0.0725640535905707,-0.0625727109491047,
-0.0538805473344791,-0.0536858997378307),.UNSPECIFIED.);
#282=B_SPLINE_CURVE_WITH_KNOTS('',3,(#26682,#26683,#26684,#26685,#26686,
#26687,#26688,#26689,#26690,#26691,#26692,#26693,#26694,#26695),
 .UNSPECIFIED.,.F.,.F.,(4,2,2,2,2,2,4),(-0.00030506004969664,0.,0.000943899264666623,
0.00572977625979271,0.0094163950019481,0.012198995415075,0.0138876784363644),
 .UNSPECIFIED.);
#283=B_SPLINE_CURVE_WITH_KNOTS('',3,(#26705,#26706,#26707,#26708,#26709,
#26710,#26711,#26712,#26713,#26714,#26715,#26716,#26717,#26718,#26719,#26720),
 .UNSPECIFIED.,.F.,.F.,(4,2,2,2,2,2,2,4),(0.0536858997405358,0.053880547337153,
0.0625727109524208,0.072564053594619,0.0859159770056253,0.0987536985036731,
0.112218387896803,0.112607088671311),.UNSPECIFIED.);
#284=B_SPLINE_CURVE_WITH_KNOTS('',3,(#26737,#26738,#26739,#26740,#26741,
#26742,#26743,#26744,#26745,#26746,#26747,#26748,#26749,#26750,#26751,#26752),
 .UNSPECIFIED.,.F.,.F.,(4,2,2,2,2,2,2,4),(-0.0143120844458313,-0.0134558136848229,
-0.0126001113738633,-0.0111102618619966,-0.00945160573383406,-0.00817883662994094,
-0.00716755165087691,-0.00685143448301955),.UNSPECIFIED.);
#285=B_SPLINE_CURVE_WITH_KNOTS('',3,(#26758,#26759,#26760,#26761,#26762,
#26763,#26764,#26765,#26766,#26767,#26768,#26769,#26770,#26771,#26772,#26773),
 .UNSPECIFIED.,.F.,.F.,(4,2,2,2,2,2,2,4),(-0.0477691295329166,-0.0476102750829768,
-0.0405164866121143,-0.0323624211366189,-0.0214657417197341,-0.0109887092118291,
0.,0.000317223787610884),.UNSPECIFIED.);
#286=B_SPLINE_CURVE_WITH_KNOTS('',3,(#27563,#27564,#27565,#27566,#27567,
#27568,#27569,#27570,#27571,#27572,#27573,#27574,#27575,#27576,#27577,#27578,
#27579,#27580),.UNSPECIFIED.,.F.,.F.,(4,2,2,2,2,2,2,2,4),(-0.43274489877026,
-0.430566610808932,-0.366750838333452,-0.304029800566765,-0.242875294955372,
-0.178422965186677,-0.116422491534204,-0.0594147705022417,-1.00000014308099E-6),
 .UNSPECIFIED.);
#287=B_SPLINE_CURVE_WITH_KNOTS('',3,(#27585,#27586,#27587,#27588,#27589,
#27590,#27591,#27592,#27593,#27594,#27595,#27596,#27597,#27598,#27599,#27600,
#27601,#27602,#27603,#27604,#27605,#27606,#27607,#27608,#27609,#27610,#27611,
#27612,#27613,#27614,#27615,#27616,#27617,#27618,#27619,#27620),
 .UNSPECIFIED.,.F.,.F.,(4,2,2,2,2,2,2,2,2,2,2,2,2,2,2,2,2,4),(-19.2450053801115,
-19.2031768304234,-19.1598456798386,-19.0949006094766,-19.0334251672637,
-18.9702316873635,-18.9060263489697,-18.8445259693451,-18.7806926247621,
-18.7178014261615,-18.6556018787519,-18.5909471802907,-18.5294501788449,
-18.4665257879972,-18.402418282567,-18.3411369020005,-18.2775557826221,
-18.2291330230763),.UNSPECIFIED.);
#288=B_SPLINE_CURVE_WITH_KNOTS('',3,(#27621,#27622,#27623,#27624,#27625,
#27626,#27627,#27628,#27629,#27630,#27631,#27632,#27633,#27634,#27635,#27636,
#27637,#27638,#27639,#27640,#27641,#27642,#27643,#27644,#27645,#27646,#27647,
#27648,#27649,#27650,#27651,#27652,#27653,#27654,#27655,#27656),
 .UNSPECIFIED.,.F.,.F.,(4,2,2,2,2,2,2,2,2,2,2,2,2,2,2,2,2,4),(-1.44203697926293,
-1.4313638992077,-1.36763608561743,-1.30534850184486,-1.24392281733326,
-1.17994358039373,-1.11838123753809,-1.05518319144789,-0.992043251713187,
-0.931149897187872,-0.867403341159369,-0.804924419349115,-0.743688850259094,
-0.679499044411844,-0.617742148113744,-0.554989179996601,-0.491622357088245,
-0.43274489877026),.UNSPECIFIED.);
#289=B_SPLINE_CURVE_WITH_KNOTS('',3,(#27661,#27662,#27663,#27664,#27665,
#27666,#27667,#27668,#27669,#27670,#27671,#27672,#27673,#27674,#27675,#27676,
#27677,#27678,#27679,#27680,#27681,#27682,#27683,#27684,#27685,#27686,#27687,
#27688,#27689,#27690,#27691,#27692,#27693,#27694,#27695,#27696),
 .UNSPECIFIED.,.F.,.F.,(4,2,2,2,2,2,2,2,2,2,2,2,2,2,2,2,2,4),(-18.2291330230763,
-18.2142764734255,-18.1522985596194,-18.0878831874444,-18.0262511910666,
-17.9635462256414,-17.8994836443016,-17.8383136315764,-17.7749377886959,
-17.7111621363704,-17.6493553372961,-17.5851256348085,-17.523253667619,
-17.460715475918,-17.3966486756835,-17.3354834665992,-17.2722627022774,
-17.2148871211445),.UNSPECIFIED.);
#290=B_SPLINE_CURVE_WITH_KNOTS('',3,(#27697,#27698,#27699,#27700,#27701,
#27702,#27703,#27704,#27705,#27706,#27707,#27708,#27709,#27710,#27711,#27712,
#27713,#27714,#27715,#27716,#27717,#27718,#27719,#27720,#27721,#27722,#27723,
#27724,#27725,#27726,#27727,#27728,#27729,#27730,#27731,#27732),
 .UNSPECIFIED.,.F.,.F.,(4,2,2,2,2,2,2,2,2,2,2,2,2,2,2,2,2,4),(-2.45150341078276,
-2.43286047511311,-2.36903133970015,-2.30696197397495,-2.24488499218074,
-2.18116000510695,-2.11982988395945,-2.05548507244458,-1.99265052578627,
-1.93176465691352,-1.86800840567019,-1.80585819717295,-1.74414477494485,
-1.6803213060518,-1.61890199565926,-1.55516382793806,-1.49220248568474,
-1.44203697926293),.UNSPECIFIED.);
#291=B_SPLINE_CURVE_WITH_KNOTS('',3,(#27737,#27738,#27739,#27740,#27741,
#27742,#27743,#27744,#27745,#27746,#27747,#27748,#27749,#27750,#27751,#27752,
#27753,#27754,#27755,#27756,#27757,#27758,#27759,#27760,#27761,#27762,#27763,
#27764,#27765,#27766,#27767,#27768,#27769,#27770,#27771,#27772,#27773,#27774),
 .UNSPECIFIED.,.F.,.F.,(4,2,2,2,2,2,2,2,2,2,2,2,2,2,2,2,2,2,4),(-17.2148871211445,
-17.2079083714811,-17.1462197339146,-17.0821193488849,-17.019918692549,
-16.9574916802273,-16.8933746296132,-16.8321170763526,-16.7689976469936,
-16.7048985425935,-16.6433013614118,-16.5793023952618,-16.5166170188716,
-16.4542691805168,-16.3894540991377,-16.3280048025785,-16.2649330315475,
-16.2007900611284,-16.1993047752053),.UNSPECIFIED.);
#292=B_SPLINE_CURVE_WITH_KNOTS('',3,(#27775,#27776,#27777,#27778,#27779,
#27780,#27781,#27782,#27783,#27784,#27785,#27786,#27787,#27788,#27789,#27790,
#27791,#27792,#27793,#27794,#27795,#27796,#27797,#27798,#27799,#27800,#27801,
#27802,#27803,#27804,#27805,#27806,#27807,#27808,#27809,#27810),
 .UNSPECIFIED.,.F.,.F.,(4,2,2,2,2,2,2,2,2,2,2,2,2,2,2,2,2,4),(-3.46293164573458,
-3.43582224646228,-3.37160540074597,-3.30981966037079,-3.24682737909425,
-3.18343959020337,-3.12235170905143,-3.05846173865086,-2.99572612090002,
-2.93445791446144,-2.86999522889465,-2.80798169069714,-2.74535920823371,
-2.68171365556681,-2.62045422247672,-2.5566456545727,-2.49388282097086,
-2.45150341078276),.UNSPECIFIED.);
#293=B_SPLINE_CURVE_WITH_KNOTS('',3,(#27815,#27816,#27817,#27818,#27819,
#27820,#27821,#27822,#27823,#27824,#27825,#27826,#27827,#27828,#27829,#27830,
#27831,#27832,#27833,#27834,#27835,#27836,#27837,#27838,#27839,#27840,#27841,
#27842,#27843,#27844,#27845,#27846,#27847,#27848,#27849,#27850),
 .UNSPECIFIED.,.F.,.F.,(4,2,2,2,2,2,2,2,2,2,2,2,2,2,2,2,2,4),(-16.1993047752053,
-16.139399623149,-16.0756819505149,-16.0126884662279,-15.9505936606462,
-15.8860511093153,-15.8245397396625,-15.7617197496252,-15.6976554447056,
-15.636446366356,-15.5729645605997,-15.5095423831343,-15.4476515691147,
-15.3833296291909,-15.3216449938471,-15.2590261184408,-15.1949889672839,
-15.1849810020995),.UNSPECIFIED.);
#294=B_SPLINE_CURVE_WITH_KNOTS('',3,(#27851,#27852,#27853,#27854,#27855,
#27856,#27857,#27858,#27859,#27860,#27861,#27862,#27863,#27864,#27865,#27866,
#27867,#27868,#27869,#27870,#27871,#27872,#27873,#27874,#27875,#27876,#27877,
#27878,#27879,#27880,#27881,#27882,#27883,#27884,#27885,#27886),
 .UNSPECIFIED.,.F.,.F.,(4,2,2,2,2,2,2,2,2,2,2,2,2,2,2,2,2,4),(-4.47360893918925,
-4.43794954459914,-4.37406242834937,-4.31257984542803,-4.24854010296684,
-4.18552550866014,-4.12458339993076,-4.06074796570392,-3.99841199290557,
-3.93680004026492,-3.87277595257713,-3.81116800361354,-3.74769502592802,
-3.68451859179219,-3.62355703375697,-3.55971906533952,-3.49720928424716,
-3.46293164573458),.UNSPECIFIED.);
#295=B_SPLINE_CURVE_WITH_KNOTS('',3,(#27891,#27892,#27893,#27894,#27895,
#27896,#27897,#27898,#27899,#27900,#27901,#27902,#27903,#27904,#27905,#27906,
#27907,#27908,#27909,#27910,#27911,#27912,#27913,#27914,#27915,#27916,#27917,
#27918,#27919,#27920,#27921,#27922,#27923,#27924,#27925,#27926),
 .UNSPECIFIED.,.F.,.F.,(4,2,2,2,2,2,2,2,2,2,2,2,2,2,2,2,2,4),(-15.1849810020995,
-15.1338530100102,-15.070559094631,-15.0066083905476,-14.9448702116096,
-14.880714276949,-14.8187558459082,-14.7562843671171,-14.6922264280455,
-14.6310595201955,-14.5679020497222,-14.5033508992441,-14.4417116096791,
-14.3776644891707,-14.3153519312524,-14.2529714041824,-14.1888475931021,
-14.1707416963743),.UNSPECIFIED.);
#296=B_SPLINE_CURVE_WITH_KNOTS('',3,(#27927,#27928,#27929,#27930,#27931,
#27932,#27933,#27934,#27935,#27936,#27937,#27938,#27939,#27940,#27941,#27942,
#27943,#27944,#27945,#27946,#27947,#27948,#27949,#27950,#27951,#27952,#27953,
#27954,#27955,#27956,#27957,#27958,#27959,#27960,#27961,#27962),
 .UNSPECIFIED.,.F.,.F.,(4,2,2,2,2,2,2,2,2,2,2,2,2,2,2,2,2,4),(-5.48535228916885,
-5.44066073025292,-5.37716695179706,-5.31599374200483,-5.25209855020388,
-5.18924548417807,-5.12804829157604,-5.06345594395374,-5.00132373767058,
-4.93893004537637,-4.87514967405474,-4.81376360203583,-4.74990140251206,
-4.68699557761332,-4.62597435119929,-4.5620951884975,-4.49987800983087,
-4.47360893918925),.UNSPECIFIED.);
#297=B_SPLINE_CURVE_WITH_KNOTS('',3,(#27967,#27968,#27969,#27970,#27971,
#27972,#27973,#27974,#27975,#27976,#27977,#27978,#27979,#27980,#27981,#27982,
#27983,#27984,#27985,#27986,#27987,#27988,#27989,#27990,#27991,#27992,#27993,
#27994,#27995,#27996,#27997,#27998,#27999,#28000,#28001,#28002),
 .UNSPECIFIED.,.F.,.F.,(4,2,2,2,2,2,2,2,2,2,2,2,2,2,2,2,2,4),(-14.1707416963743,
-14.1275575364455,-14.0644816493245,-14.0003777496193,-13.9388161694758,
-13.8748559310113,-13.8120154097725,-13.7496985264462,-13.6849190009467,
-13.6233996931089,-13.5603578496633,-13.4961841329855,-13.4348074482046,
-13.3711132207576,-13.3079206564436,-13.2458402648998,-13.1813158002758,
-13.154780839114),.UNSPECIFIED.);
#298=B_SPLINE_CURVE_WITH_KNOTS('',3,(#28003,#28004,#28005,#28006,#28007,
#28008,#28009,#28010,#28011,#28012,#28013,#28014,#28015,#28016,#28017,#28018,
#28019,#28020,#28021,#28022,#28023,#28024,#28025,#28026,#28027,#28028,#28029,
#28030,#28031,#28032,#28033,#28034,#28035,#28036,#28037,#28038),
 .UNSPECIFIED.,.F.,.F.,(4,2,2,2,2,2,2,2,2,2,2,2,2,2,2,2,2,4),(-6.49539175200228,
-6.44175461758173,-6.37869675301284,-6.31780818618473,-6.25403343173878,
-6.19164606426418,-6.13024672738864,-6.06616052832269,-6.00449767885634,
-5.94140530906691,-5.87815315446652,-5.81717609779043,-5.75336705637975,
-5.69077185590904,-5.62952948385544,-5.56521587780421,-5.50334261762044,
-5.48535228916885),.UNSPECIFIED.);
#299=B_SPLINE_CURVE_WITH_KNOTS('',3,(#28043,#28044,#28045,#28046,#28047,
#28048,#28049,#28050,#28051,#28052,#28053,#28054,#28055,#28056,#28057,#28058,
#28059,#28060,#28061,#28062,#28063,#28064,#28065,#28066,#28067,#28068,#28069,
#28070,#28071,#28072,#28073,#28074,#28075,#28076,#28077,#28078),
 .UNSPECIFIED.,.F.,.F.,(4,2,2,2,2,2,2,2,2,2,2,2,2,2,2,2,2,4),(-13.154780839114,
-13.1196948938244,-13.0568878202012,-12.9927745160496,-12.9315418600343,
-12.868067425228,-12.8044082571734,-12.7425145031164,-12.6781922176648,
-12.6163617176352,-12.5537376505848,-12.4896345068317,-12.4284379893464,
-12.3651341760799,-12.3009175828982,-12.2391582045385,-12.1749824942442,
-12.1398252878704),.UNSPECIFIED.);
#300=B_SPLINE_CURVE_WITH_KNOTS('',3,(#28079,#28080,#28081,#28082,#28083,
#28084,#28085,#28086,#28087,#28088,#28089,#28090,#28091,#28092,#28093,#28094,
#28095,#28096,#28097,#28098,#28099,#28100,#28101,#28102,#28103,#28104,#28105,
#28106,#28107,#28108,#28109,#28110,#28111,#28112,#28113,#28114),
 .UNSPECIFIED.,.F.,.F.,(4,2,2,2,2,2,2,2,2,2,2,2,2,2,2,2,2,4),(-7.50558706522749,
-7.4434856273175,-7.38066073607584,-7.31964567117951,-7.25579777663904,
-7.19366409555753,-7.13166323964892,-7.06786727378737,-7.00647046448262,
-6.94227522225779,-6.87936093702994,-6.81845608236433,-6.75466739446041,
-6.69243480618895,-6.63077645718591,-6.56686368184471,-6.50536045230073,
-6.49539175200228),.UNSPECIFIED.);
#301=B_SPLINE_CURVE_WITH_KNOTS('',3,(#28119,#28120,#28121,#28122,#28123,
#28124,#28125,#28126,#28127,#28128,#28129,#28130,#28131,#28132,#28133,#28134,
#28135,#28136,#28137,#28138,#28139,#28140,#28141,#28142,#28143,#28144,#28145,
#28146,#28147,#28148,#28149,#28150,#28151,#28152,#28153,#28154),
 .UNSPECIFIED.,.F.,.F.,(4,2,2,2,2,2,2,2,2,2,2,2,2,2,2,2,2,4),(-12.1398252878704,
-12.1128469838547,-12.0503511223232,-11.9862112217519,-11.9249500379598,
-11.861764103918,-11.7976401351988,-11.73598361746,-11.6719213824629,-11.6093387981136,
-11.5469349800063,-11.4820586087665,-11.4206376040574,-11.3575104256224,
-11.2933655333597,-11.2292834427868,-11.1662639105294,-11.1240342053348),
 .UNSPECIFIED.);
#302=B_SPLINE_CURVE_WITH_KNOTS('',3,(#28155,#28156,#28157,#28158,#28159,
#28160,#28161,#28162,#28163,#28164,#28165,#28166,#28167,#28168,#28169,#28170,
#28171,#28172,#28173,#28174,#28175,#28176,#28177,#28178,#28179,#28180,#28181,
#28182,#28183,#28184,#28185,#28186,#28187,#28188,#28189,#28190,#28191,#28192),
 .UNSPECIFIED.,.F.,.F.,(4,2,2,2,2,2,2,2,2,2,2,2,2,2,2,2,2,2,4),(-8.51705611258781,
-8.51047438623768,-8.44665403963334,-8.38410939297357,-8.32279614319828,
-8.25853933422636,-8.19671765139568,-8.13387567283019,-8.07044331417221,
-8.00932342898535,-7.94543561802143,-7.88265029342846,-7.82142233119061,
-7.75690445982659,-7.69484058642041,-7.63233160620855,-7.56862817681911,
-7.5073144426173,-7.50558706522749),.UNSPECIFIED.);
#303=B_SPLINE_CURVE_WITH_KNOTS('',3,(#28197,#28198,#28199,#28200,#28201,
#28202,#28203,#28204,#28205,#28206,#28207,#28208,#28209,#28210,#28211,#28212,
#28213,#28214,#28215,#28216,#28217,#28218,#28219,#28220,#28221,#28222,#28223,
#28224,#28225,#28226,#28227,#28228,#28229,#28230,#28231,#28232),
 .UNSPECIFIED.,.F.,.F.,(4,2,2,2,2,2,2,2,2,2,2,2,2,2,2,2,2,4),(-11.1240342053348,
-11.1049715007544,-11.0408683970359,-10.9785460178958,-10.9161742311307,
-10.85219096625,-10.7906118138308,-10.7259407224929,-10.6628544690203,-10.6017066275169,
-10.5376807557104,-10.4752825869107,-10.4132817799571,-10.3492050927119,
-10.2875415246768,-10.2234842795807,-10.1602757416615,-10.1102965696432),
 .UNSPECIFIED.);
#304=B_SPLINE_CURVE_WITH_KNOTS('',3,(#28233,#28234,#28235,#28236,#28237,
#28238,#28239,#28240,#28241,#28242,#28243,#28244,#28245,#28246,#28247,#28248,
#28249,#28250,#28251,#28252,#28253,#28254,#28255,#28256,#28257,#28258,#28259,
#28260,#28261,#28262,#28263,#28264,#28265,#28266,#28267,#28268),
 .UNSPECIFIED.,.F.,.F.,(4,2,2,2,2,2,2,2,2,2,2,2,2,2,2,2,2,4),(-9.52725242033231,
-9.51228710180808,-9.44845348442619,-9.38623386265022,-9.32443494998258,
-9.26054076930463,-9.19905317665517,-9.13521773232532,-9.07218767679157,
-9.01127714224445,-8.94747372038282,-8.88511865511398,-8.82361115858219,
-8.75956314764917,-8.6979343471348,-8.63464271854794,-8.57143574519437,
-8.51705611258781),.UNSPECIFIED.);
#305=B_SPLINE_CURVE_WITH_KNOTS('',3,(#28273,#28274,#28275,#28276,#28277,
#28278,#28279,#28280,#28281,#28282,#28283,#28284,#28285,#28286,#28287,#28288,
#28289,#28290,#28291,#28292,#28293,#28294,#28295,#28296,#28297,#28298,#28299,
#28300,#28301,#28302,#28303,#28304,#28305,#28306,#28307,#28308),
 .UNSPECIFIED.,.F.,.F.,(4,2,2,2,2,2,2,2,2,2,2,2,2,2,2,2,2,4),(-10.1102965696432,
-10.0991843775796,-10.0351913345793,-9.97266042570376,-9.91095678307518,
-9.84672895535158,-9.78492671650828,-9.72141934320778,-9.6580361697458,
-9.59689974457259,-9.53289243950799,-9.47017432877619,-9.40867125058455,
-9.3442370011338,-9.28224412700868,-9.21919366214322,-9.15558705531007,
-9.09687640456266),.UNSPECIFIED.);
#306=B_SPLINE_CURVE_WITH_KNOTS('',3,(#28309,#28310,#28311,#28312,#28313,
#28314,#28315,#28316,#28317,#28318,#28319,#28320,#28321,#28322,#28323,#28324,
#28325,#28326,#28327,#28328,#28329,#28330,#28331,#28332,#28333,#28334,#28335,
#28336,#28337,#28338,#28339,#28340,#28341,#28342,#28343,#28344),
 .UNSPECIFIED.,.F.,.F.,(4,2,2,2,2,2,2,2,2,2,2,2,2,2,2,2,2,4),(-10.5381172670408,
-10.512455978803,-10.4503254341735,-10.386510740348,-10.3255411450287,-10.2627213346113,
-10.1989245869234,-10.1376195399027,-10.0739241689982,-10.0115286955865,
-9.94947636117586,-9.88735421108905,-9.82512831769023,-9.76135256505236,
-9.69997254252333,-9.63615374965774,-9.57324861389179,-9.52725242033231),
 .UNSPECIFIED.);
#307=B_SPLINE_CURVE_WITH_KNOTS('',3,(#28349,#28350,#28351,#28352,#28353,
#28354,#28355,#28356,#28357,#28358,#28359,#28360,#28361,#28362,#28363,#28364,
#28365,#28366,#28367,#28368,#28369,#28370,#28371,#28372,#28373,#28374,#28375,
#28376,#28377,#28378,#28379,#28380,#28381,#28382,#28383,#28384,#28385,#28386),
 .UNSPECIFIED.,.F.,.F.,(4,2,2,2,2,2,2,2,2,2,2,2,2,2,2,2,2,2,4),(-9.09687640456266,
-9.09429765138321,-9.0302256031248,-8.96726887397095,-8.9058576390194,-8.84116440171671,
-8.77893131411787,-8.71622177873111,-8.65234579423566,-8.59086571160834,
-8.52685699401383,-8.46386280799012,-8.40267113289702,-8.33864297752146,
-8.27634241271939,-8.2141493879631,-8.15018297227031,-8.08862181773403,
-8.08262706977625),.UNSPECIFIED.);
#308=B_SPLINE_CURVE_WITH_KNOTS('',3,(#28387,#28388,#28389,#28390,#28391,
#28392,#28393,#28394,#28395,#28396,#28397,#28398,#28399,#28400,#28401,#28402,
#28403,#28404,#28405,#28406,#28407,#28408,#28409,#28410,#28411,#28412,#28413,
#28414,#28415,#28416,#28417,#28418,#28419,#28420,#28421,#28422),
 .UNSPECIFIED.,.F.,.F.,(4,2,2,2,2,2,2,2,2,2,2,2,2,2,2,2,2,4),(-11.5476264878665,
-11.5140365460968,-11.4516308740854,-11.3878716449922,-11.3269918026019,
-11.2639182524274,-11.2004369463522,-11.1389245305944,-11.07500084939,-11.013417671742,
-10.9511772470223,-10.8874131737632,-10.8265367108085,-10.7636167982201,
-10.6995586349995,-10.6381630855281,-10.5743673266148,-10.5381172670408),
 .UNSPECIFIED.);
#309=B_SPLINE_CURVE_WITH_KNOTS('',3,(#28427,#28428,#28429,#28430,#28431,
#28432,#28433,#28434,#28435,#28436,#28437,#28438,#28439,#28440,#28441,#28442,
#28443,#28444,#28445,#28446,#28447,#28448,#28449,#28450,#28451,#28452,#28453,
#28454,#28455,#28456,#28457,#28458,#28459,#28460,#28461,#28462),
 .UNSPECIFIED.,.F.,.F.,(4,2,2,2,2,2,2,2,2,2,2,2,2,2,2,2,2,4),(-8.08262706977625,
-8.02421455182451,-7.96113392805235,-7.90005770458101,-7.83609144286503,
-7.77369497498638,-7.71184945932058,-7.64776923316301,-7.58610448703455,
-7.52229170167221,-7.45907012529655,-7.39801598821222,-7.33406637134758,
-7.27151783754628,-7.20993747384233,-7.14568653069794,-7.08386471745399,
-7.07010568792935),.UNSPECIFIED.);
#310=B_SPLINE_CURVE_WITH_KNOTS('',3,(#28463,#28464,#28465,#28466,#28467,
#28468,#28469,#28470,#28471,#28472,#28473,#28474,#28475,#28476,#28477,#28478,
#28479,#28480,#28481,#28482,#28483,#28484,#28485,#28486,#28487,#28488,#28489,
#28490,#28491,#28492,#28493,#28494,#28495,#28496,#28497,#28498),
 .UNSPECIFIED.,.F.,.F.,(4,2,2,2,2,2,2,2,2,2,2,2,2,2,2,2,2,4),(-12.5583011318705,
-12.5164244272338,-12.453533904535,-12.3896340325225,-12.3284282946859,
-12.2649006882095,-12.202302571561,-12.1404006409781,-12.0760554349159,
-12.0148482976973,-11.9522249338035,-11.8884216857418,-11.8274324792701,
-11.7641552830532,-11.701169280429,-11.6394872633689,-11.5753795396612,
-11.5476264878665),.UNSPECIFIED.);
#311=B_SPLINE_CURVE_WITH_KNOTS('',3,(#28503,#28504,#28505,#28506,#28507,
#28508,#28509,#28510,#28511,#28512,#28513,#28514,#28515,#28516,#28517,#28518,
#28519,#28520,#28521,#28522,#28523,#28524,#28525,#28526,#28527,#28528,#28529,
#28530,#28531,#28532,#28533,#28534,#28535,#28536,#28537,#28538),
 .UNSPECIFIED.,.F.,.F.,(4,2,2,2,2,2,2,2,2,2,2,2,2,2,2,2,2,4),(-7.07010568792935,
-7.02057195526808,-6.95715837040495,-6.89602168015075,-6.83204054447954,
-6.76928656991371,-6.7078697716623,-6.64339382293125,-6.58136387292713,
-6.51848925069081,-6.45483602060775,-6.3935087439113,-6.32944430613884,
-6.26643455412798,-6.20506961813476,-6.14031704292197,-6.07803016863274,
-6.05626210410768),.UNSPECIFIED.);
#312=B_SPLINE_CURVE_WITH_KNOTS('',3,(#28539,#28540,#28541,#28542,#28543,
#28544,#28545,#28546,#28547,#28548,#28549,#28550,#28551,#28552,#28553,#28554,
#28555,#28556,#28557,#28558,#28559,#28560,#28561,#28562,#28563,#28564,#28565,
#28566,#28567,#28568,#28569,#28570,#28571,#28572,#28573,#28574),
 .UNSPECIFIED.,.F.,.F.,(4,2,2,2,2,2,2,2,2,2,2,2,2,2,2,2,2,4),(-13.5700232395142,
-13.5204005870663,-13.4573318747156,-13.3933719339399,-13.3318427510029,
-13.2679060883571,-13.2060132812835,-13.1437505760427,-13.0798539406011,
-13.0188264204508,-12.9558764789665,-12.8919955376263,-12.8305697425558,
-12.766747094191,-12.7044120458901,-12.6422420703319,-12.5776085442114,
-12.5583011318705),.UNSPECIFIED.);
#313=B_SPLINE_CURVE_WITH_KNOTS('',3,(#28579,#28580,#28581,#28582,#28583,
#28584,#28585,#28586,#28587,#28588,#28589,#28590,#28591,#28592,#28593,#28594,
#28595,#28596,#28597,#28598,#28599,#28600,#28601,#28602,#28603,#28604,#28605,
#28606,#28607,#28608,#28609,#28610,#28611,#28612,#28613,#28614),
 .UNSPECIFIED.,.F.,.F.,(4,2,2,2,2,2,2,2,2,2,2,2,2,2,2,2,2,4),(-6.05626210410768,
-6.0154519013265,-5.9515138295235,-5.88997569337269,-5.82594853894846,-5.7628879405073,
-5.70170531265335,-5.63766078512489,-5.57529108892424,-5.51318619075399,
-5.44914331646863,-5.38751051846565,-5.32327540580219,-5.26010879987577,
-5.19901056374118,-5.13501235853817,-5.07252669067762,-5.04250930940443),
 .UNSPECIFIED.);
#314=B_SPLINE_CURVE_WITH_KNOTS('',3,(#28615,#28616,#28617,#28618,#28619,
#28620,#28621,#28622,#28623,#28624,#28625,#28626,#28627,#28628,#28629,#28630,
#28631,#28632,#28633,#28634,#28635,#28636,#28637,#28638,#28639,#28640,#28641,
#28642,#28643,#28644,#28645,#28646,#28647,#28648,#28649,#28650),
 .UNSPECIFIED.,.F.,.F.,(4,2,2,2,2,2,2,2,2,2,2,2,2,2,2,2,2,4),(-14.5813080464973,
-14.5229842167791,-14.459524148473,-14.3965799254724,-14.3347283766724,
-14.2704415484857,-14.2090567993869,-14.1464813701105,-14.0826089233366,
-14.0216048982894,-13.9583649586076,-13.8949584508584,-13.8332940872334,
-13.769210006081,-13.7076189535549,-13.6452271481187,-13.5813660136001,
-13.5700232395142),.UNSPECIFIED.);
#315=B_SPLINE_CURVE_WITH_KNOTS('',3,(#28655,#28656,#28657,#28658,#28659,
#28660,#28661,#28662,#28663,#28664,#28665,#28666,#28667,#28668,#28669,#28670,
#28671,#28672,#28673,#28674,#28675,#28676,#28677,#28678,#28679,#28680,#28681,
#28682,#28683,#28684,#28685,#28686,#28687,#28688,#28689,#28690),
 .UNSPECIFIED.,.F.,.F.,(4,2,2,2,2,2,2,2,2,2,2,2,2,2,2,2,2,4),(-5.04250930940443,
-5.01074345740576,-4.94656642853249,-4.88481091988587,-4.82114792736413,
-4.75782191979311,-4.69670993316011,-4.63271182641902,-4.57005488216266,
-4.50850272047019,-4.4441354654514,-4.38220455481827,-4.31902895774606,
-4.25549371142046,-4.19426107834615,-4.13021367387332,-4.06733312302916,
-4.02900754571855),.UNSPECIFIED.);
#316=B_SPLINE_CURVE_WITH_KNOTS('',3,(#28691,#28692,#28693,#28694,#28695,
#28696,#28697,#28698,#28699,#28700,#28701,#28702,#28703,#28704,#28705,#28706,
#28707,#28708,#28709,#28710,#28711,#28712,#28713,#28714,#28715,#28716,#28717,
#28718,#28719,#28720,#28721,#28722,#28723,#28724,#28725,#28726,#28727,#28728),
 .UNSPECIFIED.,.F.,.F.,(4,2,2,2,2,2,2,2,2,2,2,2,2,2,2,2,2,2,4),(-15.5933221971989,
-15.5875677904679,-15.5261531677509,-15.4623393509046,-15.400265719406,
-15.3381128208409,-15.2742269043841,-15.2131662822886,-15.1503208065578,
-15.0864546018284,-15.0251184153014,-14.9613922317184,-14.8987956903211,
-14.8367073456883,-14.7721651536426,-14.7108788500126,-14.6480683038418,
-14.5841343915024,-14.5813080464973),.UNSPECIFIED.);
#317=B_SPLINE_CURVE_WITH_KNOTS('',3,(#28733,#28734,#28735,#28736,#28737,
#28738,#28739,#28740,#28741,#28742,#28743,#28744,#28745,#28746,#28747,#28748,
#28749,#28750,#28751,#28752,#28753,#28754,#28755,#28756,#28757,#28758,#28759,
#28760,#28761,#28762,#28763,#28764,#28765,#28766,#28767,#28768),
 .UNSPECIFIED.,.F.,.F.,(4,2,2,2,2,2,2,2,2,2,2,2,2,2,2,2,2,4),(-4.02900754571855,
-4.0059062389982,-3.94129539215301,-3.87913881741449,-3.81634060720317,
-3.75254945348995,-3.69114962308604,-3.62718800769495,-3.56428259058608,
-3.50310844301288,-3.43912597478557,-3.37691614892503,-3.31467179696546,
-3.25080355834965,-3.18933527194429,-3.12480362707408,-3.06182973481643,
-3.01586943876209),.UNSPECIFIED.);
#318=B_SPLINE_CURVE_WITH_KNOTS('',3,(#28769,#28770,#28771,#28772,#28773,
#28774,#28775,#28776,#28777,#28778,#28779,#28780,#28781,#28782,#28783,#28784,
#28785,#28786,#28787,#28788,#28789,#28790,#28791,#28792,#28793,#28794,#28795,
#28796,#28797,#28798,#28799,#28800,#28801,#28802,#28803,#28804),
 .UNSPECIFIED.,.F.,.F.,(4,2,2,2,2,2,2,2,2,2,2,2,2,2,2,2,2,4),(-16.6035198604699,
-16.5900454824747,-16.52837749622,-16.4642869299382,-16.4028347554628,-16.3404414845704,
-16.2766395839102,-16.2157277579415,-16.152662237515,-16.0889611903744,
-16.0274466316654,-15.9635229009172,-15.9018003282277,-15.8395553329516,
-15.7757339163795,-15.71479381237,-15.6518656052688,-15.5933221971989),
 .UNSPECIFIED.);
#319=B_SPLINE_CURVE_WITH_KNOTS('',3,(#28809,#28810,#28811,#28812,#28813,
#28814,#28815,#28816,#28817,#28818,#28819,#28820,#28821,#28822,#28823,#28824,
#28825,#28826,#28827,#28828,#28829,#28830,#28831,#28832,#28833,#28834,#28835,
#28836,#28837,#28838,#28839,#28840,#28841,#28842,#28843,#28844),
 .UNSPECIFIED.,.F.,.F.,(4,2,2,2,2,2,2,2,2,2,2,2,2,2,2,2,2,4),(-3.01586943876209,
-3.00079724181661,-2.93689043293634,-2.8746030456085,-2.81272692241491,
-2.74876349342228,-2.68720912181028,-2.62328856932311,-2.56019082819264,
-2.49921153393853,-2.43533598225039,-2.37291425081546,-2.31133185138697,
-2.24721568730844,-2.18552114055543,-2.12214682151061,-2.05887309443656,
-2.00453087624746),.UNSPECIFIED.);
#320=B_SPLINE_CURVE_WITH_KNOTS('',3,(#28845,#28846,#28847,#28848,#28849,
#28850,#28851,#28852,#28853,#28854,#28855,#28856,#28857,#28858,#28859,#28860,
#28861,#28862,#28863,#28864,#28865,#28866,#28867,#28868,#28869,#28870,#28871,
#28872,#28873,#28874,#28875,#28876,#28877,#28878,#28879,#28880),
 .UNSPECIFIED.,.F.,.F.,(4,2,2,2,2,2,2,2,2,2,2,2,2,2,2,2,2,4),(-17.614935493873,
-17.5934598904259,-17.53133403337,-17.4667494645793,-17.4055260732277,-17.3426789621963,
-17.2787689742008,-17.2175980676138,-17.1541078739038,-17.0913554027581,
-17.0294828842969,-16.9651711475964,-16.9038888570392,-16.8412938681442,
-16.7774636347221,-16.7164761842175,-16.653222186963,-16.6035198604699),
 .UNSPECIFIED.);
#321=B_SPLINE_CURVE_WITH_KNOTS('',3,(#28886,#28887,#28888,#28889,#28890,
#28891,#28892,#28893,#28894,#28895,#28896,#28897,#28898,#28899,#28900,#28901,
#28902,#28903,#28904,#28905,#28906,#28907,#28908,#28909,#28910,#28911,#28912,
#28913,#28914,#28915,#28916,#28917),.UNSPECIFIED.,.F.,.F.,(4,2,2,2,2,2,
2,2,2,2,2,2,2,2,2,4),(-19.4936808899958,-19.4531550473275,-19.4114253894815,
-19.3480658590082,-19.2850241322855,-19.2232628932131,-19.159072502976,
-19.0976657032011,-19.0351800920759,-18.9713461232385,-18.910393411917,
-18.8472396492887,-18.7837058034619,-18.7221163760458,-18.6581123837969,
-18.6261649225256),.UNSPECIFIED.);
#322=B_SPLINE_CURVE_WITH_KNOTS('',3,(#28920,#28921,#28922,#28923,#28924,
#28925,#28926,#28927,#28928,#28929,#28930,#28931,#28932,#28933,#28934,#28935,
#28936,#28937,#28938,#28939,#28940,#28941,#28942,#28943,#28944,#28945,#28946,
#28947,#28948,#28949,#28950,#28951,#28952,#28953),.UNSPECIFIED.,.F.,.F.,
(4,2,2,2,2,2,2,2,2,2,2,2,2,2,2,2,4),(-0.991954268502835,-0.92969776175528,
-0.866808936262966,-0.805726881798867,-0.741810702793368,-0.679614012179091,
-0.617539964427152,-0.553679664627321,-0.49222081736718,-0.427944533954764,
-0.364967508943842,-0.303997772933001,-0.240141878760337,-0.177847495603767,
-0.116117953761281,-0.0578271827732781,-9.99999998252399E-7),
 .UNSPECIFIED.);
#323=B_SPLINE_CURVE_WITH_KNOTS('',3,(#29557,#29558,#29559,#29560,#29561,
#29562,#29563,#29564,#29565,#29566,#29567,#29568,#29569,#29570,#29571,#29572,
#29573,#29574,#29575,#29576,#29577,#29578,#29579,#29580,#29581,#29582,#29583,
#29584,#29585,#29586,#29587,#29588),.UNSPECIFIED.,.F.,.F.,(4,2,2,2,2,2,
2,2,2,2,2,2,2,2,2,4),(1.0000000159313E-6,0.184001326101672,0.37041664464277,
0.703290139702188,1.03440506548376,1.36773974881136,1.69865455171767,2.03244840671975,
2.36317397254373,2.6974230132541,3.02797037146041,3.3626688271678,3.69304907229932,
4.02818958292247,4.35841380142651,4.64135684187533),.UNSPECIFIED.);
#324=B_SPLINE_CURVE_WITH_KNOTS('',3,(#29591,#29592,#29593,#29594,#29595,
#29596,#29597,#29598,#29599,#29600,#29601,#29602,#29603,#29604,#29605,#29606,
#29607,#29608,#29609,#29610,#29611,#29612,#29613,#29614,#29615,#29616,#29617,
#29618),.UNSPECIFIED.,.F.,.F.,(4,2,2,2,2,2,2,2,2,2,2,2,2,4),(14.0669063991451,
14.1284264825117,14.4671173829221,14.7937484791654,15.1326547393244,15.4593625495219,
15.7984769197192,16.1252697919598,16.4645851145556,16.7914700330379,17.1309792827163,
17.4579619797361,17.7485763441689,18.0394413523531),.UNSPECIFIED.);
#325=B_SPLINE_CURVE_WITH_KNOTS('',3,(#29623,#29624,#29625,#29626,#29627,
#29628,#29629,#29630,#29631,#29632,#29633,#29634,#29635,#29636,#29637,#29638,
#29639,#29640,#29641,#29642,#29643,#29644,#29645,#29646,#29647,#29648,#29649,
#29650,#29651,#29652,#29653,#29654,#29655,#29656,#29657,#29658),
 .UNSPECIFIED.,.F.,.F.,(4,2,2,2,2,2,2,2,2,2,2,2,2,2,2,2,2,4),(4.64135684187533,
4.69398762946712,5.02406690378143,5.36006416228109,5.6900092970561,6.0264189975231,
6.35624067954145,6.69305109308465,7.02275977360977,7.35995854918521,7.68956440436171,
8.02713873558435,8.35665163351959,8.69458841162062,9.02401788581675,9.35169718603101,
9.69247573073726,10.0050542561348),.UNSPECIFIED.);
#326=B_SPLINE_CURVE_WITH_KNOTS('',3,(#29659,#29660,#29661,#29662,#29663,
#29664,#29665,#29666,#29667,#29668,#29669,#29670,#29671,#29672,#29673,#29674,
#29675,#29676,#29677,#29678,#29679,#29680,#29681,#29682,#29683,#29684,#29685,
#29686,#29687,#29688,#29689,#29690,#29691,#29692,#29693,#29694),
 .UNSPECIFIED.,.F.,.F.,(4,2,2,2,2,2,2,2,2,2,2,2,2,2,2,2,2,4),(8.70719789233371,
8.81570165061824,9.1524157175717,9.47892443720727,9.81590840352668,10.1423689843966,
10.4796170049242,10.8060509235,11.1435567243114,11.4699838356931,11.8077407934984,
12.1341792602608,12.4721804795241,12.7986467381769,13.1368851247795,13.4633938864294,
13.8018622169238,14.0669063991451),.UNSPECIFIED.);
#327=B_SPLINE_CURVE_WITH_KNOTS('',3,(#29699,#29700,#29701,#29702,#29703,
#29704,#29705,#29706,#29707,#29708,#29709,#29710,#29711,#29712,#29713,#29714,
#29715,#29716,#29717,#29718,#29719,#29720,#29721,#29722,#29723,#29724,#29725,
#29726,#29727,#29728,#29729,#29730,#29731,#29732,#29733,#29734),
 .UNSPECIFIED.,.F.,.F.,(4,2,2,2,2,2,2,2,2,2,2,2,2,2,2,2,2,4),(10.0050542561348,
10.0202666236202,10.361182715358,10.6890843397369,11.0301335185425,11.358144772174,
11.6993228356638,12.0274424289947,12.3687454254136,12.696971928326,13.0383961484681,
13.3667280305269,13.7082699987937,14.0367056635557,14.3783621283825,14.7068999423348,
15.0486678661882,15.3747761103741),.UNSPECIFIED.);
#328=B_SPLINE_CURVE_WITH_KNOTS('',3,(#29735,#29736,#29737,#29738,#29739,
#29740,#29741,#29742,#29743,#29744,#29745,#29746,#29747,#29748,#29749,#29750,
#29751,#29752,#29753,#29754,#29755,#29756,#29757,#29758,#29759,#29760,#29761,
#29762,#29763,#29764,#29765,#29766,#29767,#29768,#29769,#29770),
 .UNSPECIFIED.,.F.,.F.,(4,2,2,2,2,2,2,2,2,2,2,2,2,2,2,2,2,4),(3.34852080740999,
3.51541382366282,3.84983510106026,4.1776416565033,4.51235510680904,4.83990488875393,
5.17491070933339,5.50223095942833,5.83752839411276,6.16464663854683,6.50023401625068,
6.82717773172898,7.16305251610975,7.48984881036069,7.82600765901454,8.15268297405058,
8.48912180554802,8.70719789233371),.UNSPECIFIED.);
#329=B_SPLINE_CURVE_WITH_KNOTS('',3,(#30067,#30068,#30069,#30070,#30071,
#30072,#30073,#30074,#30075,#30076),.UNSPECIFIED.,.F.,.F.,(4,2,2,2,4),(-1.08763065698974,
-0.805155960498027,-0.481178691573332,-0.239177070179376,-1.00000002545286E-6),
 .UNSPECIFIED.);
#330=B_SPLINE_CURVE_WITH_KNOTS('',3,(#30079,#30080,#30081,#30082,#30083,
#30084,#30085,#30086,#30087,#30088,#30089,#30090,#30091,#30092,#30093,#30094,
#30095,#30096,#30097,#30098,#30099,#30100,#30101,#30102,#30103,#30104,#30105,
#30106,#30107,#30108),.UNSPECIFIED.,.F.,.F.,(4,2,2,2,2,2,2,2,2,2,2,2,2,
2,4),(-22.8315979776072,-22.6468550995409,-22.4614144304526,-22.1495542369066,
-21.8319967613863,-21.5198417749621,-21.2025574749825,-20.8900847176457,
-20.5730704622723,-20.2602584541901,-19.9435101871991,-19.6303391935868,
-19.3138519590932,-19.0003042009862,-18.8651569875978),.UNSPECIFIED.);
#331=B_SPLINE_CURVE_WITH_KNOTS('',3,(#30113,#30114,#30115,#30116,#30117,
#30118,#30119,#30120,#30121,#30122,#30123,#30124,#30125,#30126,#30127,#30128,
#30129,#30130,#30131,#30132,#30133,#30134,#30135,#30136,#30137,#30138,#30139,
#30140,#30141,#30142,#30143,#30144,#30145,#30146,#30147,#30148,#30149,#30150),
 .UNSPECIFIED.,.F.,.F.,(4,2,2,2,2,2,2,2,2,2,2,2,2,2,2,2,2,2,4),(-6.19306152073892,
-6.19215501284973,-5.88122082091077,-5.558699659647,-5.24769703205706,-4.92497158059589,
-4.61389148723222,-4.29096837903147,-3.9798031422975,-3.65668890928387,
-3.34543210441171,-3.02213314223365,-2.71077949168461,-2.38730203042346,
-2.07584729564655,-1.75219737570318,-1.44063824902751,-1.11682170183935,
-1.08763065698974),.UNSPECIFIED.);
#332=B_SPLINE_CURVE_WITH_KNOTS('',3,(#30151,#30152,#30153,#30154,#30155,
#30156,#30157,#30158,#30159,#30160,#30161,#30162,#30163,#30164,#30165,#30166,
#30167,#30168,#30169,#30170,#30171,#30172,#30173,#30174,#30175,#30176,#30177,
#30178,#30179,#30180,#30181,#30182,#30183,#30184,#30185,#30186),
 .UNSPECIFIED.,.F.,.F.,(4,2,2,2,2,2,2,2,2,2,2,2,2,2,2,2,2,4),(-18.8651569875978,
-18.6840721358553,-18.3701318810007,-18.0541483667636,-17.7398022919276,
-17.424059979304,-17.1092970137406,-16.7937878340886,-16.4785992730197,
-16.1633145468654,-15.84769404259,-15.5326245591325,-15.2165680717643,-14.9017041714821,
-14.5852098835831,-14.2705415421437,-13.9536097423191,-13.7714023393986),
 .UNSPECIFIED.);
#333=B_SPLINE_CURVE_WITH_KNOTS('',3,(#30191,#30192,#30193,#30194,#30195,
#30196,#30197,#30198,#30199,#30200,#30201,#30202,#30203,#30204,#30205,#30206,
#30207,#30208,#30209,#30210,#30211,#30212,#30213,#30214,#30215,#30216,#30217,
#30218,#30219,#30220,#30221,#30222,#30223,#30224,#30225,#30226),
 .UNSPECIFIED.,.F.,.F.,(4,2,2,2,2,2,2,2,2,2,2,2,2,2,2,2,2,4),(-11.2955132668756,
-11.2499663755103,-10.9350810181394,-10.618816702694,-10.3035134580392,
-9.98748241249118,-9.6766841977884,-9.35552796049665,-9.04474773802309,
-8.72334793560915,-8.4125672990213,-8.09093012940668,-7.78013227347285,
-7.45826415837377,-7.14743390049163,-6.82534141835785,-6.51446518933045,
-6.19306152073892),.UNSPECIFIED.);
#334=B_SPLINE_CURVE_WITH_KNOTS('',3,(#30227,#30228,#30229,#30230,#30231,
#30232,#30233,#30234,#30235,#30236,#30237,#30238,#30239,#30240,#30241,#30242,
#30243,#30244,#30245,#30246,#30247,#30248,#30249,#30250,#30251,#30252,#30253,
#30254,#30255,#30256,#30257,#30258,#30259,#30260,#30261,#30262),
 .UNSPECIFIED.,.F.,.F.,(4,2,2,2,2,2,2,2,2,2,2,2,2,2,2,2,2,4),(-13.7714023393986,
-13.6391266540991,-13.321759595108,-13.0074512547913,-12.6896529919331,
-12.375508772851,-12.0572849883311,-11.7432942164274,-11.4246520351327,
-11.1024784175165,-10.7919151734175,-10.469543341878,-10.1588960412222,
-9.83633253271426,-9.52559460027536,-9.20284582000664,-8.89201184020883,
-8.67522927952334),.UNSPECIFIED.);
#335=B_SPLINE_CURVE_WITH_KNOTS('',3,(#30268,#30269,#30270,#30271,#30272,
#30273,#30274,#30275,#30276,#30277,#30278,#30279,#30280,#30281,#30282,#30283,
#30284,#30285,#30286,#30287,#30288,#30289,#30290,#30291,#30292,#30293),
 .UNSPECIFIED.,.F.,.F.,(4,2,2,2,2,2,2,2,2,2,2,2,4),(-3.57460038523497,-3.48941625606424,
-3.17761372514257,-2.85332018035678,-2.54140882943066,-2.21698644756211,
-1.90496726499796,-1.5804197501514,-1.26829388464313,-0.943624715683776,
-0.631393435474488,-0.306605874008126,0.),.UNSPECIFIED.);
#336=B_SPLINE_CURVE_WITH_KNOTS('',3,(#30296,#30297,#30298,#30299,#30300,
#30301,#30302,#30303,#30304,#30305,#30306,#30307,#30308,#30309,#30310,#30311,
#30312,#30313,#30314,#30315,#30316,#30317,#30318,#30319,#30320,#30321),
 .UNSPECIFIED.,.F.,.F.,(4,2,2,2,2,2,2,2,2,2,2,2,4),(-19.9682012621818,-19.7098781597989,
-19.4484728160962,-19.1373255636262,-18.8175881446957,-18.5062982349599,
-18.1868340849252,-17.8753757400517,-17.5561870800245,-17.2445342177348,
-16.9256224526336,-16.613748987607,-16.3969931861447),.UNSPECIFIED.);
#337=B_SPLINE_CURVE_WITH_KNOTS('',3,(#30323,#30324,#30325,#30326,#30327,
#30328,#30329,#30330,#30331,#30332,#30333,#30334,#30335,#30336,#30337,#30338,
#30339,#30340,#30341,#30342,#30343,#30344,#30345,#30346,#30347,#30348,#30349,
#30350,#30351,#30352,#30353,#30354,#30355,#30356,#30357,#30358),
 .UNSPECIFIED.,.F.,.F.,(4,2,2,2,2,2,2,2,2,2,2,2,2,2,2,2,2,4),(-16.3969931861447,
-16.2951146586955,-15.9829948163869,-15.6646375641271,-15.3522460653515,
-15.0341645906407,-14.7214770909201,-14.4036691687269,-14.0906626928763,
-13.7731251587965,-13.4597782402757,-13.1425070036526,-12.8287999308234,
-12.5117900008011,-12.1977050268771,-11.8809505507568,-11.5664720626041,
-11.2955132668756),.UNSPECIFIED.);
#338=B_SPLINE_CURVE_WITH_KNOTS('',3,(#30359,#30360,#30361,#30362,#30363,
#30364,#30365,#30366,#30367,#30368,#30369,#30370,#30371,#30372,#30373,#30374,
#30375,#30376,#30377,#30378,#30379,#30380,#30381,#30382,#30383,#30384,#30385,
#30386,#30387,#30388,#30389,#30390,#30391,#30392,#30393,#30394),
 .UNSPECIFIED.,.F.,.F.,(4,2,2,2,2,2,2,2,2,2,2,2,2,2,2,2,2,4),(-8.67522927952334,
-8.56908403168542,-8.258149640719,-7.93504886100084,-7.6240106387303,-7.30074273855771,
-6.98959810256552,-6.6661687109744,-6.35491581460173,-6.03133032761751,
-5.71996796341123,-5.39623153639831,-5.08475904596485,-4.76087658920983,
-4.44929378011827,-4.1252699572342,-3.81357702730685,-3.57460038523497),
 .UNSPECIFIED.);
#339=B_SPLINE_CURVE_WITH_KNOTS('',3,(#30546,#30547,#30548,#30549,#30550,
#30551,#30552,#30553,#30554,#30555,#30556,#30557),.UNSPECIFIED.,.F.,.F.,
(4,2,2,2,2,4),(-0.792142372778785,-0.591597628920338,-0.397953596192907,
-0.200017601361334,-0.098121308975255,-1.00000001490574E-6),
 .UNSPECIFIED.);
#340=B_SPLINE_CURVE_WITH_KNOTS('',3,(#30558,#30559,#30560,#30561,#30562,
#30563,#30564,#30565,#30566,#30567),.UNSPECIFIED.,.F.,.F.,(4,2,2,2,4),(-0.755948032479872,
-0.604406814456052,-0.40541099667635,-0.208806710351552,0.),
 .UNSPECIFIED.);
#341=B_SPLINE_CURVE_WITH_KNOTS('',3,(#30879,#30880,#30881,#30882,#30883,
#30884,#30885,#30886,#30887,#30888,#30889,#30890,#30891,#30892,#30893,#30894,
#30895,#30896,#30897,#30898,#30899,#30900,#30901,#30902),.UNSPECIFIED.,
 .F.,.F.,(4,2,2,2,2,2,2,2,2,2,2,4),(1.0000000253329E-6,0.266750129365986,
0.536833672900569,0.866300625148748,1.19957484557901,1.52866431091697,1.8622200413073,
2.19095299525438,2.5247943758972,2.8531936331742,3.18732382651167,3.34852080740999),
 .UNSPECIFIED.);
#342=B_SPLINE_CURVE_WITH_KNOTS('',3,(#31162,#31163,#31164,#31165,#31166,
#31167,#31168,#31169,#31170,#31171,#31172,#31173,#31174,#31175,#31176,#31177,
#31178,#31179,#31180,#31181),.UNSPECIFIED.,.F.,.F.,(4,2,2,2,2,2,2,2,2,4),
(15.3747761103741,15.3773061828803,15.7191827319993,16.0479199119144,16.3899024459424,
16.7187368726242,17.060822934254,17.3897234764764,17.7317277368266,18.062135331452),
 .UNSPECIFIED.);
#343=B_SPLINE_CURVE_WITH_KNOTS('',3,(#32336,#32337,#32338,#32339,#32340,
#32341,#32342,#32343,#32344,#32345,#32346,#32347,#32348,#32349,#32350,#32351,
#32352,#32353,#32354,#32355,#32356,#32357,#32358,#32359,#32360,#32361,#32362,
#32363,#32364,#32365,#32366,#32367,#32368,#32369,#32370,#32371,#32372,#32373),
 .UNSPECIFIED.,.F.,.F.,(4,2,2,2,2,2,2,2,2,2,2,2,2,2,2,2,2,2,4),(-2.00453087624746,
-1.99784530757748,-1.9339539081977,-1.87134356757002,-1.80995795666769,
-1.74563396690078,-1.68374745704052,-1.6208256951135,-1.55732738492814,
-1.49614332060061,-1.43218556118532,-1.3693353892712,-1.30803770782599,
-1.24345350991551,-1.18132562328791,-1.11874004258405,-1.05497136296553,
-0.99359471855428,-0.991954268502835),.UNSPECIFIED.);
#344=B_SPLINE_CURVE_WITH_KNOTS('',3,(#32896,#32897,#32898,#32899,#32900,
#32901,#32902,#32903,#32904,#32905,#32906,#32907,#32908,#32909,#32910,#32911,
#32912,#32913,#32914,#32915,#32916,#32917,#32918,#32919,#32920,#32921,#32922,
#32923,#32924,#32925,#32926,#32927,#32928,#32929,#32930,#32931),
 .UNSPECIFIED.,.F.,.F.,(4,2,2,2,2,2,2,2,2,2,2,2,2,2,2,2,2,4),(-18.6261649225256,
-18.5964689905192,-18.5341509277396,-18.4703139576672,-18.4093686462651,
-18.346370722227,-18.2822619886212,-18.2207916693756,-18.1569179891035,
-18.0949490218438,-18.0327431791459,-17.9688572712294,-17.9078222340396,
-17.8449266834194,-17.7810584978724,-17.7196802765616,-17.6559086764456,
-17.614935493873),.UNSPECIFIED.);
#345=B_SPLINE_CURVE_WITH_KNOTS('',3,(#33030,#33031,#33032,#33033,#33034,
#33035,#33036,#33037,#33038,#33039,#33040,#33041,#33042,#33043,#33044,#33045,
#33046,#33047,#33048),.UNSPECIFIED.,.F.,.F.,(4,1,1,1,1,1,1,1,1,1,1,1,1,
1,1,1,4),(0.,0.064429890715421,0.126529667073554,0.186743666835525,0.245897683478137,
0.304053106820992,0.362195516217047,0.420654638852463,0.480330856318868,
0.540662876085596,0.600743511343268,0.661981856833518,0.724480055372708,
0.789067141037209,0.856333336778513,0.926362064011592,1.),.UNSPECIFIED.);
#346=B_SPLINE_CURVE_WITH_KNOTS('',3,(#33050,#33051,#33052,#33053,#33054,
#33055,#33056,#33057,#33058,#33059,#33060,#33061,#33062,#33063,#33064,#33065,
#33066,#33067,#33068),.UNSPECIFIED.,.F.,.F.,(4,1,1,1,1,1,1,1,1,1,1,1,1,
1,1,1,4),(0.,0.0619654006870562,0.122121905638296,0.180988496849837,0.239933216451894,
0.299905831106524,0.359988847476984,0.421775741741642,0.486575826421121,
0.551534804619736,0.615017542759975,0.677258616661654,0.739729962362713,
0.803050102662949,0.866495132015699,0.931973474177149,1.),.UNSPECIFIED.);
#347=B_SPLINE_CURVE_WITH_KNOTS('',3,(#33070,#33071,#33072,#33073,#33074,
#33075,#33076,#33077,#33078,#33079,#33080,#33081,#33082,#33083,#33084),
 .UNSPECIFIED.,.F.,.F.,(4,1,1,1,1,1,1,1,1,1,1,1,4),(0.,0.110802643801324,
0.212829202347773,0.306101309823115,0.390647321116006,0.46692446936085,
0.534481039284033,0.593586940965671,0.644557004508714,0.736200452629367,
0.825024025618864,0.911985584829753,1.),.UNSPECIFIED.);
#348=B_SPLINE_CURVE_WITH_KNOTS('',3,(#33096,#33097,#33098,#33099,#33100,
#33101,#33102,#33103,#33104,#33105,#33106,#33107,#33108,#33109,#33110),
 .UNSPECIFIED.,.F.,.F.,(4,1,1,1,1,1,1,1,1,1,1,1,4),(0.,0.0987013748863702,
0.195670680385855,0.292419992908961,0.391339286967469,0.444458741764931,
0.504224579154748,0.570347591406357,0.642913825979479,0.722289816523959,
0.807922721202247,0.900470366297794,1.),.UNSPECIFIED.);
#349=B_SPLINE_CURVE_WITH_KNOTS('',3,(#33112,#33113,#33114,#33115,#33116,
#33117,#33118,#33119,#33120,#33121,#33122,#33123,#33124,#33125,#33126,#33127,
#33128,#33129,#33130),.UNSPECIFIED.,.F.,.F.,(4,1,1,1,1,1,1,1,1,1,1,1,1,
1,1,1,4),(0.,0.0694796363669832,0.136525003539142,0.200800892873422,0.263983206913328,
0.325711144761188,0.38727051407573,0.449492780531563,0.51295519576285,0.576266397070109,
0.637574966831173,0.697901098424494,0.757558279411561,0.81658750436506,
0.876645756608308,0.937285872938128,1.),.UNSPECIFIED.);
#350=B_SPLINE_CURVE_WITH_KNOTS('',3,(#33132,#33133,#33134,#33135,#33136,
#33137,#33138,#33139,#33140,#33141,#33142,#33143,#33144,#33145,#33146,#33147,
#33148,#33149,#33150),.UNSPECIFIED.,.F.,.F.,(4,1,1,1,1,1,1,1,1,1,1,1,1,
1,1,1,4),(0.,0.0687907943906199,0.135103289431132,0.198978674310652,0.261904299780862,
0.323494969367974,0.385195377966055,0.446969238740777,0.509764776703136,
0.572250568847369,0.633405175661155,0.693251162921754,0.752583162785671,
0.812579266153423,0.873275084920192,0.93554994289503,1.),.UNSPECIFIED.);
#351=B_SPLINE_CURVE_WITH_KNOTS('',3,(#33192,#33193,#33194,#33195,#33196,
#33197,#33198,#33199,#33200,#33201,#33202,#33203,#33204,#33205,#33206,#33207,
#33208,#33209,#33210),.UNSPECIFIED.,.F.,.F.,(4,1,1,1,1,1,1,1,1,1,1,1,1,
1,1,1,4),(0.,0.0619654006870562,0.122121905638296,0.180988496849837,0.239933216451894,
0.299905831106524,0.359988847476984,0.421775741741642,0.486575826421121,
0.551534804619736,0.615017542759975,0.677258616661654,0.739729962362713,
0.803050102662949,0.866495132015699,0.931973474177149,1.),.UNSPECIFIED.);
#352=B_SPLINE_CURVE_WITH_KNOTS('',3,(#33244,#33245,#33246,#33247,#33248,
#33249,#33250,#33251,#33252,#33253,#33254,#33255,#33256,#33257,#33258),
 .UNSPECIFIED.,.F.,.F.,(4,1,1,1,1,1,1,1,1,1,1,1,4),(0.,0.110802643801324,
0.212829202347773,0.306101309823115,0.390647321116006,0.46692446936085,
0.534481039284033,0.593586940965671,0.644557004508714,0.736200452629367,
0.825024025618864,0.911985584829753,1.),.UNSPECIFIED.);
#353=B_SPLINE_CURVE_WITH_KNOTS('',3,(#33311,#33312,#33313,#33314,#33315,
#33316,#33317,#33318,#33319,#33320,#33321,#33322,#33323,#33324,#33325),
 .UNSPECIFIED.,.F.,.F.,(4,1,1,1,1,1,1,1,1,1,1,1,4),(0.,0.0987013748863702,
0.195670680385855,0.292419992908961,0.391339286967469,0.444458741764931,
0.504224579154748,0.570347591406357,0.642913825979479,0.722289816523959,
0.807922721202247,0.900470366297794,1.),.UNSPECIFIED.);
#354=B_SPLINE_CURVE_WITH_KNOTS('',3,(#33366,#33367,#33368,#33369,#33370,
#33371,#33372,#33373,#33374,#33375,#33376,#33377,#33378,#33379,#33380,#33381,
#33382,#33383,#33384),.UNSPECIFIED.,.F.,.F.,(4,1,1,1,1,1,1,1,1,1,1,1,1,
1,1,1,4),(0.,0.0694796363669832,0.136525003539142,0.200800892873422,0.263983206913328,
0.325711144761188,0.38727051407573,0.449492780531563,0.51295519576285,0.576266397070109,
0.637574966831173,0.697901098424494,0.757558279411561,0.81658750436506,
0.876645756608308,0.937285872938128,1.),.UNSPECIFIED.);
#355=B_SPLINE_CURVE_WITH_KNOTS('',3,(#33425,#33426,#33427,#33428,#33429,
#33430,#33431,#33432,#33433,#33434,#33435,#33436,#33437,#33438,#33439,#33440,
#33441,#33442,#33443),.UNSPECIFIED.,.F.,.F.,(4,1,1,1,1,1,1,1,1,1,1,1,1,
1,1,1,4),(0.,0.0687907943906199,0.135103289431132,0.198978674310652,0.261904299780862,
0.323494969367974,0.385195377966055,0.446969238740777,0.509764776703136,
0.572250568847369,0.633405175661155,0.693251162921754,0.752583162785671,
0.812579266153423,0.873275084920192,0.93554994289503,1.),.UNSPECIFIED.);
#356=B_SPLINE_CURVE_WITH_KNOTS('',3,(#33487,#33488,#33489,#33490,#33491,
#33492,#33493,#33494,#33495,#33496,#33497,#33498,#33499,#33500,#33501,#33502,
#33503,#33504,#33505),.UNSPECIFIED.,.F.,.F.,(4,1,1,1,1,1,1,1,1,1,1,1,1,
1,1,1,4),(0.,0.064429890715421,0.126529667073554,0.186743666835525,0.245897683478137,
0.304053106820992,0.362195516217047,0.420654638852463,0.480330856318868,
0.540662876085596,0.600743511343268,0.661981856833518,0.724480055372708,
0.789067141037209,0.856333336778513,0.926362064011592,1.),.UNSPECIFIED.);
#357=B_SPLINE_CURVE_WITH_KNOTS('',3,(#33774,#33775,#33776,#33777,#33778,
#33779,#33780,#33781,#33782,#33783,#33784,#33785,#33786,#33787,#33788,#33789,
#33790,#33791,#33792,#33793,#33794,#33795),.UNSPECIFIED.,.F.,.F.,(4,2,2,
2,2,2,2,2,2,2,4),(13.142711462932,13.1579818167511,13.2217062873234,13.2838063508681,
13.3455231362043,13.4092932791525,13.4706620157354,13.5344323685447,13.5973377391588,
13.657787218639,13.7194997062356),.UNSPECIFIED.);
#358=B_SPLINE_CURVE_WITH_KNOTS('',3,(#33800,#33801,#33802,#33803,#33804,
#33805,#33806,#33807,#33808,#33809,#33810,#33811,#33812,#33813,#33814,#33815,
#33816,#33817,#33818,#33819,#33820,#33821,#33822,#33823,#33824,#33825,#33826,
#33827,#33828,#33829,#33830,#33831,#33832,#33833,#33834,#33835),
 .UNSPECIFIED.,.F.,.F.,(4,2,2,2,2,2,2,2,2,2,2,2,2,2,2,2,2,4),(0.,0.0359582530012615,
0.0731837666941684,0.137235112949865,0.198838631694034,0.261200010699037,
0.32504770195871,0.386000749088701,0.44904001871335,0.513045713500326,0.574549640221195,
0.638459422251555,0.700373110277162,0.762611164523284,0.826498988256686,
0.887523750164669,0.950449850339167,1.01090153686108),.UNSPECIFIED.);
#359=B_SPLINE_CURVE_WITH_KNOTS('',3,(#33836,#33837,#33838,#33839,#33840,
#33841,#33842,#33843,#33844,#33845,#33846,#33847,#33848,#33849,#33850,#33851,
#33852,#33853,#33854,#33855,#33856,#33857,#33858,#33859,#33860,#33861,#33862,
#33863,#33864,#33865,#33866,#33867,#33868,#33869,#33870,#33871),
 .UNSPECIFIED.,.F.,.F.,(4,2,2,2,2,2,2,2,2,2,2,2,2,2,2,2,2,4),(12.1323404141985,
12.1556573917594,12.2200847211504,12.2820653373017,12.3447227235141,12.4083318674643,
12.4695568071821,12.5333442349376,12.5960689705528,12.6570830861283,12.7215467187269,
12.7835529410482,12.8457066305132,12.9093617916751,12.9706262125415,13.0343352675459,
13.0971204251574,13.142711462932),.UNSPECIFIED.);
#360=B_SPLINE_CURVE_WITH_KNOTS('',3,(#33876,#33877,#33878,#33879,#33880,
#33881,#33882,#33883,#33884,#33885,#33886,#33887,#33888,#33889,#33890,#33891,
#33892,#33893,#33894,#33895,#33896,#33897,#33898,#33899,#33900,#33901,#33902,
#33903,#33904,#33905,#33906,#33907,#33908,#33909,#33910,#33911,#33912,#33913),
 .UNSPECIFIED.,.F.,.F.,(4,2,2,2,2,2,2,2,2,2,2,2,2,2,2,2,2,2,4),(1.01090153686108,
1.01432125508311,1.07572564016303,1.13952547317396,1.20189435909138,1.26404402197446,
1.32865534671711,1.38984758335372,1.45271798203398,1.51661625113869,1.57780436811715,
1.64131392739509,1.70396013741204,1.76584688882252,1.83017529548686,1.89140309254637,
1.95401157225196,2.01781915854794,2.02253426878796),.UNSPECIFIED.);
#361=B_SPLINE_CURVE_WITH_KNOTS('',3,(#33914,#33915,#33916,#33917,#33918,
#33919,#33920,#33921,#33922,#33923,#33924,#33925,#33926,#33927,#33928,#33929,
#33930,#33931,#33932,#33933,#33934,#33935,#33936,#33937,#33938,#33939,#33940,
#33941,#33942,#33943,#33944,#33945,#33946,#33947,#33948,#33949),
 .UNSPECIFIED.,.F.,.F.,(4,2,2,2,2,2,2,2,2,2,2,2,2,2,2,2,2,4),(11.1214864347725,
11.1534488115465,11.2174503566185,11.2790374548038,11.3425714444984,11.4057227010986,
11.4666734207028,11.5305054568745,11.5929885337885,11.6543942371259,11.7185819722754,
11.7803406867599,11.843382214289,11.9067390545548,11.9678030898047,12.0316809910961,
12.0943838071615,12.1323404141985),.UNSPECIFIED.);
#362=B_SPLINE_CURVE_WITH_KNOTS('',3,(#33954,#33955,#33956,#33957,#33958,
#33959,#33960,#33961,#33962,#33963,#33964,#33965,#33966,#33967,#33968,#33969,
#33970,#33971,#33972,#33973,#33974,#33975,#33976,#33977,#33978,#33979,#33980,
#33981,#33982,#33983,#33984,#33985,#33986,#33987,#33988,#33989),
 .UNSPECIFIED.,.F.,.F.,(4,2,2,2,2,2,2,2,2,2,2,2,2,2,2,2,2,4),(2.02253426878796,
2.07880223700639,2.14206634117737,2.20511331401215,2.26678551297205,2.33088212000521,
2.39225776527954,2.45465411191018,2.51842320109549,2.57930873182499,2.64237446317126,
2.70592714775301,2.76743537711405,2.83135393252775,2.89298050251894,2.95521750681276,
3.01899659602717,3.03218372263281),.UNSPECIFIED.);
#363=B_SPLINE_CURVE_WITH_KNOTS('',3,(#33990,#33991,#33992,#33993,#33994,
#33995,#33996,#33997,#33998,#33999,#34000,#34001,#34002,#34003,#34004,#34005,
#34006,#34007,#34008,#34009,#34010,#34011,#34012,#34013,#34014,#34015,#34016,
#34017,#34018,#34019,#34020,#34021,#34022,#34023,#34024,#34025),
 .UNSPECIFIED.,.F.,.F.,(4,2,2,2,2,2,2,2,2,2,2,2,2,2,2,2,2,4),(10.1102829969334,
10.1512710656532,10.2150405861368,10.2764168243332,10.3402833928885,10.4031768398644,
10.464210597169,10.5280949109509,10.5902986361653,10.6522671409988,10.716138589806,
10.7776067824405,10.8417158948343,10.9047115085251,10.9656552090866,11.0294904215152,
11.0918061543416,11.1214864347725),.UNSPECIFIED.);
#364=B_SPLINE_CURVE_WITH_KNOTS('',3,(#34030,#34031,#34032,#34033,#34034,
#34035,#34036,#34037,#34038,#34039,#34040,#34041,#34042,#34043,#34044,#34045,
#34046,#34047,#34048,#34049,#34050,#34051,#34052,#34053,#34054,#34055,#34056,
#34057,#34058,#34059,#34060,#34061,#34062,#34063,#34064,#34065),
 .UNSPECIFIED.,.F.,.F.,(4,2,2,2,2,2,2,2,2,2,2,2,2,2,2,2,2,4),(3.03218372263281,
3.07988992137784,3.14280768521512,3.20694447876217,3.26834173965761,3.33213864733873,
3.39410160796508,3.45623492856705,3.52006950765413,3.581065702496,3.643889407597,
3.70770538153846,3.76901632572646,3.83271726992244,3.89517799562774,3.95723784182379,
4.02175232938853,4.04294907391778),.UNSPECIFIED.);
#365=B_SPLINE_CURVE_WITH_KNOTS('',3,(#34066,#34067,#34068,#34069,#34070,
#34071,#34072,#34073,#34074,#34075,#34076,#34077,#34078,#34079,#34080,#34081,
#34082,#34083,#34084,#34085,#34086,#34087,#34088,#34089,#34090,#34091,#34092,
#34093,#34094,#34095,#34096,#34097,#34098,#34099,#34100,#34101),
 .UNSPECIFIED.,.F.,.F.,(4,2,2,2,2,2,2,2,2,2,2,2,2,2,2,2,2,4),(9.09888760056311,
9.1486061892843,9.21185845597294,9.27284452328484,9.3366736185903,9.39926683177369,
9.46054865914562,9.52485851951026,9.58672926579225,9.6494821976632,9.71297048300282,
9.77413960104805,9.8380482486443,9.90089339572085,9.96211589511406,10.0266983935914,
10.0888222946518,10.1102829969334),.UNSPECIFIED.);
#366=B_SPLINE_CURVE_WITH_KNOTS('',3,(#34106,#34107,#34108,#34109,#34110,
#34111,#34112,#34113,#34114,#34115,#34116,#34117,#34118,#34119,#34120,#34121,
#34122,#34123,#34124,#34125,#34126,#34127,#34128,#34129,#34130,#34131,#34132,
#34133,#34134,#34135,#34136,#34137,#34138,#34139,#34140,#34141),
 .UNSPECIFIED.,.F.,.F.,(4,2,2,2,2,2,2,2,2,2,2,2,2,2,2,2,2,4),(4.04294907391778,
4.08295248441981,4.14573340606041,4.20960220268779,4.27071419165295,4.33414048671887,
4.3969237015339,4.45873747459545,4.52298680052707,4.58426283261112,4.64679908242436,
4.71059608911083,4.77154071334328,4.83473784914837,4.89796160798484,4.95957841423839,
5.02361460467017,5.05338907499331),.UNSPECIFIED.);
#367=B_SPLINE_CURVE_WITH_KNOTS('',3,(#34142,#34143,#34144,#34145,#34146,
#34147,#34148,#34149,#34150,#34151,#34152,#34153,#34154,#34155,#34156,#34157,
#34158,#34159,#34160,#34161,#34162,#34163,#34164,#34165,#34166,#34167,#34168,
#34169,#34170,#34171,#34172,#34173,#34174,#34175,#34176,#34177),
 .UNSPECIFIED.,.F.,.F.,(4,2,2,2,2,2,2,2,2,2,2,2,2,2,2,2,2,4),(8.08870409001179,
8.14726255440374,8.21018942134961,8.27112892082392,8.33494956046087,8.3971931878043,
8.45891604108485,8.52283831070216,8.58435148775943,8.64805373114709,8.7111177098161,
8.77202855807641,8.83582950764207,8.89822120139655,8.9596733109505,9.02376220375112,
9.08542860886895,9.09888760056311),.UNSPECIFIED.);
#368=B_SPLINE_CURVE_WITH_KNOTS('',3,(#34182,#34183,#34184,#34185,#34186,
#34187,#34188,#34189,#34190,#34191,#34192,#34193,#34194,#34195,#34196,#34197,
#34198,#34199,#34200,#34201,#34202,#34203,#34204,#34205,#34206,#34207,#34208,
#34209,#34210,#34211,#34212,#34213,#34214,#34215,#34216,#34217),
 .UNSPECIFIED.,.F.,.F.,(4,2,2,2,2,2,2,2,2,2,2,2,2,2,2,2,2,4),(5.05338907499331,
5.08507620655147,5.14741861117407,5.21119465800221,5.27207967609426,5.33509582780477,
5.39885641679272,5.46032770589982,5.52420548109823,5.58595101557381,5.64815344503229,
5.71195588741959,5.77288385429669,5.83577070173323,5.90013604798391,5.96151561074328,
6.02529220384508,6.06339547208752),.UNSPECIFIED.);
#369=B_SPLINE_CURVE_WITH_KNOTS('',3,(#34218,#34219,#34220,#34221,#34222,
#34223,#34224,#34225,#34226,#34227,#34228,#34229,#34230,#34231,#34232,#34233,
#34234,#34235,#34236,#34237,#34238,#34239,#34240,#34241,#34242,#34243,#34244,
#34245,#34246,#34247,#34248,#34249,#34250,#34251,#34252,#34253,#34254,#34255),
 .UNSPECIFIED.,.F.,.F.,(4,2,2,2,2,2,2,2,2,2,2,2,2,2,2,2,2,2,4),(7.07669856726943,
7.07954003474363,7.1434735852899,7.20628315126754,7.26756956135512,7.33211069661312,
7.39419805791722,7.45679558005713,7.52052067995683,7.58185584046079,7.64572141384328,
7.70856576164337,7.76962609572472,7.83351139916469,7.89566314676714,7.95773731224237,
8.02154988815528,8.08296333620691,8.08870409001179),.UNSPECIFIED.);
#370=B_SPLINE_CURVE_WITH_KNOTS('',3,(#34260,#34261,#34262,#34263,#34264,
#34265,#34266,#34267,#34268,#34269,#34270,#34271,#34272,#34273,#34274,#34275,
#34276,#34277,#34278,#34279,#34280,#34281,#34282,#34283,#34284,#34285,#34286,
#34287,#34288,#34289,#34290,#34291,#34292,#34293,#34294,#34295),
 .UNSPECIFIED.,.F.,.F.,(4,2,2,2,2,2,2,2,2,2,2,2,2,2,2,2,2,4),(6.06339547208752,
6.08739865938769,6.14951759655391,6.21339102568026,6.27445189976627,6.3372644413378,
6.40111747590033,6.46242451331744,6.52611972557013,6.58876676321737,6.65082781566915,
6.71534028879468,6.77664248685867,6.83942599924069,6.90335733851185,6.96448924397403,
7.02753578823382,7.07536902408054),.UNSPECIFIED.);
#371=B_SPLINE_CURVE_WITH_KNOTS('',3,(#34296,#34297,#34298,#34299,#34300,
#34301,#34302,#34303,#34304,#34305,#34306,#34307,#34308,#34309,#34310,#34311,
#34312,#34313,#34314,#34315,#34316,#34317,#34318,#34319,#34320,#34321,#34322,
#34323,#34324,#34325,#34326,#34327,#34328,#34329,#34330,#34331),
 .UNSPECIFIED.,.F.,.F.,(4,2,2,2,2,2,2,2,2,2,2,2,2,2,2,2,2,4),(6.06541653120124,
6.07677442400661,6.140635558073,6.20302675441035,6.26461868394941,6.32870208754262,
6.39036582549154,6.45377413212297,6.5170133202156,6.57801697113455,6.64188924343672,
6.70446387260813,6.76584913304758,6.83013508929954,6.89198582955554,6.95493147688094,
7.01839062339183,7.07669856726943),.UNSPECIFIED.);
#372=B_SPLINE_CURVE_WITH_KNOTS('',3,(#34336,#34337,#34338,#34339,#34340,
#34341,#34342,#34343,#34344,#34345,#34346,#34347,#34348,#34349,#34350,#34351,
#34352,#34353,#34354,#34355,#34356,#34357,#34358,#34359,#34360,#34361,#34362,
#34363,#34364,#34365,#34366,#34367,#34368,#34369,#34370,#34371),
 .UNSPECIFIED.,.F.,.F.,(4,2,2,2,2,2,2,2,2,2,2,2,2,2,2,2,2,4),(7.07536902408054,
7.08855245102283,7.15246092273268,7.21482540085779,7.27657501529124,7.34062459821103,
7.402258864083,7.46593663852235,7.52913183820682,7.59014144323236,7.6540402424552,
7.7165647897316,7.77806368679493,7.84229209213344,7.90409104519249,7.96726276848113,
8.03065710497116,8.08707212644807),.UNSPECIFIED.);
#373=B_SPLINE_CURVE_WITH_KNOTS('',3,(#34372,#34373,#34374,#34375,#34376,
#34377,#34378,#34379,#34380,#34381,#34382,#34383,#34384,#34385,#34386,#34387,
#34388,#34389,#34390,#34391,#34392,#34393,#34394,#34395,#34396,#34397,#34398,
#34399,#34400,#34401,#34402,#34403,#34404,#34405,#34406,#34407),
 .UNSPECIFIED.,.F.,.F.,(4,2,2,2,2,2,2,2,2,2,2,2,2,2,2,2,2,4),(5.05358007064663,
5.07526698797775,5.13742262368034,5.20203867290101,5.26327685292802,5.32615387985161,
5.39008500223115,5.45128337214047,5.51423293972763,5.57526080610153,5.63915760440498,
5.70141990187991,5.76331389421934,5.82725008327323,5.88877883217346,5.95274084875297,
6.01580899199089,6.06541653120124),.UNSPECIFIED.);
#374=B_SPLINE_CURVE_WITH_KNOTS('',3,(#34412,#34413,#34414,#34415,#34416,
#34417,#34418,#34419,#34420,#34421,#34422,#34423,#34424,#34425,#34426,#34427,
#34428,#34429,#34430,#34431,#34432,#34433,#34434,#34435,#34436,#34437,#34438,
#34439,#34440,#34441,#34442,#34443,#34444,#34445,#34446,#34447,#34448,#34449),
 .UNSPECIFIED.,.F.,.F.,(4,2,2,2,2,2,2,2,2,2,2,2,2,2,2,2,2,2,4),(8.08707212644807,
8.09176525665677,8.15570300420656,8.2184404959072,8.27979205065832,8.34425311543039,
8.40626742353619,8.46903842955182,8.53267905944031,8.59399344981126,8.65802246642909,
8.72102276848788,8.78233953906217,8.84708446711847,8.90936257261165,8.97185664997878,
9.03578847048786,9.0973198504176,9.10077482354646),.UNSPECIFIED.);
#375=B_SPLINE_CURVE_WITH_KNOTS('',3,(#34450,#34451,#34452,#34453,#34454,
#34455,#34456,#34457,#34458,#34459,#34460,#34461,#34462,#34463,#34464,#34465,
#34466,#34467,#34468,#34469,#34470,#34471,#34472,#34473,#34474,#34475,#34476,
#34477,#34478,#34479,#34480,#34481,#34482,#34483,#34484,#34485),
 .UNSPECIFIED.,.F.,.F.,(4,2,2,2,2,2,2,2,2,2,2,2,2,2,2,2,2,4),(4.04194870124897,
4.07186646906384,4.1342195762872,4.19808356758159,4.25905380820392,4.32208652116032,
4.38619220152751,4.44769467094645,4.51160206611549,4.57357977415333,4.63581766762807,
4.69972829162907,4.76078357675388,4.82371100529867,4.88760423328709,4.94901258493515,
5.01281576269777,5.05358007064663),.UNSPECIFIED.);
#376=B_SPLINE_CURVE_WITH_KNOTS('',3,(#34490,#34491,#34492,#34493,#34494,
#34495,#34496,#34497,#34498,#34499,#34500,#34501,#34502,#34503,#34504,#34505,
#34506,#34507,#34508,#34509,#34510,#34511,#34512,#34513,#34514,#34515,#34516,
#34517,#34518,#34519,#34520,#34521,#34522,#34523,#34524,#34525),
 .UNSPECIFIED.,.F.,.F.,(4,2,2,2,2,2,2,2,2,2,2,2,2,2,2,2,2,4),(9.10077482354646,
9.16132248678141,9.22437885995756,9.28552855679668,9.34954759714026,9.41191457245069,
9.47395340314661,9.53799567643849,9.59962706543561,9.6637604846617,9.72693064242749,
9.78800913033544,9.85198827170404,9.91447921930853,9.97620780906414,10.0403923367931,
10.1021540483061,10.1138813028186),.UNSPECIFIED.);
#377=B_SPLINE_CURVE_WITH_KNOTS('',3,(#34526,#34527,#34528,#34529,#34530,
#34531,#34532,#34533,#34534,#34535,#34536,#34537,#34538,#34539,#34540,#34541,
#34542,#34543,#34544,#34545,#34546,#34547,#34548,#34549,#34550,#34551,#34552,
#34553,#34554,#34555,#34556,#34557,#34558,#34559,#34560,#34561),
 .UNSPECIFIED.,.F.,.F.,(4,2,2,2,2,2,2,2,2,2,2,2,2,2,2,2,2,4),(3.03058177228639,
3.06878888879999,3.13153509824144,3.19544728706079,3.25654971334623,3.31994938600095,
3.38299624598465,3.4447952445736,3.50902532068632,3.57044982999391,3.63297336418729,
3.69683682410905,3.75781984354876,3.821011153871,3.88454527977345,3.94616971252482,
4.01021045952113,4.04194870124897),.UNSPECIFIED.);
#378=B_SPLINE_CURVE_WITH_KNOTS('',3,(#34566,#34567,#34568,#34569,#34570,
#34571,#34572,#34573,#34574,#34575,#34576,#34577,#34578,#34579,#34580,#34581,
#34582,#34583,#34584,#34585,#34586,#34587,#34588,#34589,#34590,#34591,#34592,
#34593,#34594,#34595,#34596,#34597,#34598,#34599,#34600,#34601),
 .UNSPECIFIED.,.F.,.F.,(4,2,2,2,2,2,2,2,2,2,2,2,2,2,2,2,2,4),(10.1138813028186,
10.1657257783372,10.2290626094574,10.2901697019842,10.354155562403,10.416825378446,
10.4783374500112,10.5427199165038,10.6046642836855,10.6677630192165,10.7313158447778,
10.7925589963334,10.8566014704575,10.9195020342268,10.9809047381247,11.0455381116102,
11.1077150533666,11.1275070958942),.UNSPECIFIED.);
#379=B_SPLINE_CURVE_WITH_KNOTS('',3,(#34602,#34603,#34604,#34605,#34606,
#34607,#34608,#34609,#34610,#34611,#34612,#34613,#34614,#34615,#34616,#34617,
#34618,#34619,#34620,#34621,#34622,#34623,#34624,#34625,#34626,#34627,#34628,
#34629,#34630,#34631,#34632,#34633,#34634,#34635,#34636,#34637),
 .UNSPECIFIED.,.F.,.F.,(4,2,2,2,2,2,2,2,2,2,2,2,2,2,2,2,2,4),(2.01959218604488,
2.06541546347494,2.12825385027516,2.19265393585692,2.25399031389628,2.31772144326577,
2.37983677511548,2.44191320609392,2.50575994370993,2.5668051915514,2.62957581345711,
2.69340170507181,2.75467017069393,2.81832480001291,2.88099397655741,2.94301771886783,
3.00749040232631,3.03058177228639),.UNSPECIFIED.);
#380=B_SPLINE_CURVE_WITH_KNOTS('',3,(#34642,#34643,#34644,#34645,#34646,
#34647,#34648,#34649,#34650,#34651,#34652,#34653,#34654,#34655,#34656,#34657,
#34658,#34659,#34660,#34661,#34662,#34663,#34664,#34665,#34666,#34667,#34668,
#34669,#34670,#34671,#34672,#34673,#34674,#34675,#34676,#34677),
 .UNSPECIFIED.,.F.,.F.,(4,2,2,2,2,2,2,2,2,2,2,2,2,2,2,2,2,4),(11.1275070958942,
11.1704537304032,11.2342688483924,11.2956910839699,11.3596585420614,11.4225901153166,
11.4837561576735,11.5477438342631,11.6099809376208,11.6721838169566,11.7360824974812,
11.7975793132747,11.862033730474,11.9250424842215,11.9860793785899,12.0499980505855,
12.1123215932317,12.1402573446881),.UNSPECIFIED.);
#381=B_SPLINE_CURVE_WITH_KNOTS('',3,(#34678,#34679,#34680,#34681,#34682,
#34683,#34684,#34685,#34686,#34687,#34688,#34689,#34690,#34691,#34692,#34693,
#34694,#34695,#34696,#34697,#34698,#34699,#34700,#34701,#34702,#34703,#34704,
#34705,#34706,#34707,#34708,#34709,#34710,#34711,#34712,#34713),
 .UNSPECIFIED.,.F.,.F.,(4,2,2,2,2,2,2,2,2,2,2,2,2,2,2,2,2,4),(1.01041293968269,
1.06459532413738,1.12773186594428,1.1909758101729,1.25253688832545,1.31651426807939,
1.37796756271407,1.4402543169856,1.50399348106341,1.56484253694405,1.62780397062662,
1.69159377589592,1.75301550684636,1.81684104028362,1.87858830448784,1.94074155682194,
2.00451236612964,2.01959218604488),.UNSPECIFIED.);
#382=B_SPLINE_CURVE_WITH_KNOTS('',3,(#34720,#34721,#34722,#34723,#34724,
#34725,#34726,#34727),.UNSPECIFIED.,.F.,.F.,(4,2,2,4),(13.151979181519,
13.1772505756377,13.2268757105544,13.2769541484665),.UNSPECIFIED.);
#383=B_SPLINE_CURVE_WITH_KNOTS('',3,(#35563,#35564,#35565,#35566,#35567,
#35568,#35569,#35570,#35571,#35572,#35573,#35574,#35575,#35576,#35577,#35578,
#35579,#35580,#35581,#35582,#35583,#35584,#35585,#35586,#35587,#35588,#35589,
#35590,#35591,#35592,#35593,#35594,#35595,#35596,#35597,#35598),
 .UNSPECIFIED.,.F.,.F.,(4,2,2,2,2,2,2,2,2,2,2,2,2,2,2,2,2,4),(12.1402573446881,
12.1741660806478,12.2381689628595,12.2997603383981,12.3636114787066,12.4267523742039,
12.4877509879086,12.5516454501077,12.6141119167696,12.6756763354339,12.7398406522336,
12.8015803756614,12.8648977514758,12.9282223899383,12.9892859123381,13.0532037605178,
13.1158669759719,13.151979181519),.UNSPECIFIED.);
#384=B_SPLINE_CURVE_WITH_KNOTS('',3,(#35952,#35953,#35954,#35955,#35956,
#35957,#35958,#35959,#35960,#35961,#35962,#35963,#35964,#35965,#35966,#35967,
#35968,#35969,#35970,#35971,#35972,#35973,#35974,#35975,#35976,#35977,#35978,
#35979,#35980,#35981,#35982,#35983,#35984,#35985,#35986,#35987),
 .UNSPECIFIED.,.F.,.F.,(4,2,2,2,2,2,2,2,2,2,2,2,2,2,2,2,2,4),(0.,0.062854565099621,
0.126484087138076,0.188938677080355,0.250931183419829,0.315374552221337,
0.376541583571281,0.439254841233545,0.503075030045385,0.564126285197331,
0.62748646183889,0.690277756336167,0.752029883476157,0.8162141093586,0.877470009247812,
0.939944443819231,1.00369893667666,1.01041293968269),.UNSPECIFIED.);
#385=SPHERICAL_SURFACE('',#18134,0.5);
#386=SPHERICAL_SURFACE('',#18138,0.5);
#387=SPHERICAL_SURFACE('',#18271,0.25);
#388=SPHERICAL_SURFACE('',#18275,0.25);
#389=SPHERICAL_SURFACE('',#18279,0.25);
#390=SPHERICAL_SURFACE('',#18283,0.25);
#391=SPHERICAL_SURFACE('',#18287,0.25);
#392=SPHERICAL_SURFACE('',#18291,0.25);
#393=SPHERICAL_SURFACE('',#18295,0.25);
#394=SPHERICAL_SURFACE('',#18299,0.25);
#395=SPHERICAL_SURFACE('',#18303,0.25);
#396=SPHERICAL_SURFACE('',#18307,0.25);
#397=SPHERICAL_SURFACE('',#18396,0.25);
#398=SPHERICAL_SURFACE('',#18408,0.25);
#399=SPHERICAL_SURFACE('',#18428,0.25);
#400=SPHERICAL_SURFACE('',#18445,0.25);
#401=SPHERICAL_SURFACE('',#18448,0.25);
#402=SPHERICAL_SURFACE('',#18468,0.25);
#403=SPHERICAL_SURFACE('',#18482,0.25);
#404=SPHERICAL_SURFACE('',#18499,0.25);
#405=SPHERICAL_SURFACE('',#18502,0.25);
#406=SPHERICAL_SURFACE('',#18517,0.25);
#407=(
BOUNDED_SURFACE()
B_SPLINE_SURFACE(2,2,((#25054,#25055,#25056),(#25057,#25058,#25059),(#25060,
#25061,#25062)),.UNSPECIFIED.,.F.,.F.,.F.)
B_SPLINE_SURFACE_WITH_KNOTS((3,3),(3,3),(-1.57079632679491,1.51262184115385E-31),
(-3.14159265358979,-1.57079632679489),.UNSPECIFIED.)
GEOMETRIC_REPRESENTATION_ITEM()
RATIONAL_B_SPLINE_SURFACE(((1.,0.707106781186547,1.),(0.707106781186636,
0.500000000000062,0.707106781186636),(1.,0.707106781186547,1.)))
REPRESENTATION_ITEM('')
SURFACE()
);
#408=(
BOUNDED_SURFACE()
B_SPLINE_SURFACE(2,2,((#25105,#25106,#25107),(#25108,#25109,#25110),(#25111,
#25112,#25113)),.UNSPECIFIED.,.F.,.F.,.F.)
B_SPLINE_SURFACE_WITH_KNOTS((3,3),(3,3),(-1.5707963267949,4.00000000000002E-15),
(-1.5707963267949,8.88178419700128E-15),.UNSPECIFIED.)
GEOMETRIC_REPRESENTATION_ITEM()
RATIONAL_B_SPLINE_SURFACE(((1.,0.707106781186544,1.),(0.707106781186621,
0.50000000000005,0.707106781186621),(1.,0.707106781186544,1.)))
REPRESENTATION_ITEM('')
SURFACE()
);
#409=(
BOUNDED_SURFACE()
B_SPLINE_SURFACE(2,2,((#27320,#27321,#27322,#27323,#27324,#27325,#27326,
#27327,#27328),(#27329,#27330,#27331,#27332,#27333,#27334,#27335,#27336,
#27337),(#27338,#27339,#27340,#27341,#27342,#27343,#27344,#27345,#27346)),
 .UNSPECIFIED.,.F.,.T.,.F.)
B_SPLINE_SURFACE_WITH_KNOTS((3,3),(3,2,2,2,3),(-7.86407345739089E-15,1.57079632679491),
(-3.14159265358979,-1.5707963267949,0.,1.5707963267949,3.14159265358979),
 .UNSPECIFIED.)
GEOMETRIC_REPRESENTATION_ITEM()
RATIONAL_B_SPLINE_SURFACE(((1.,0.707106781186548,1.,0.707106781186548,1.,
0.707106781186548,1.,0.707106781186548,1.),(0.707106781186533,0.499999999999989,
0.707106781186533,0.499999999999989,0.707106781186533,0.499999999999989,
0.707106781186533,0.499999999999989,0.707106781186533),(1.,0.707106781186548,
1.,0.707106781186548,1.,0.707106781186548,1.,0.707106781186548,1.)))
REPRESENTATION_ITEM('')
SURFACE()
);
#410=(
BOUNDED_SURFACE()
B_SPLINE_SURFACE(2,2,((#27354,#27355,#27356,#27357,#27358,#27359,#27360,
#27361,#27362),(#27363,#27364,#27365,#27366,#27367,#27368,#27369,#27370,
#27371),(#27372,#27373,#27374,#27375,#27376,#27377,#27378,#27379,#27380)),
 .UNSPECIFIED.,.F.,.T.,.F.)
B_SPLINE_SURFACE_WITH_KNOTS((3,3),(3,2,2,2,3),(-7.86407345739086E-15,1.57079632679491),
(-3.14159265358979,-1.5707963267949,0.,1.5707963267949,3.14159265358979),
 .UNSPECIFIED.)
GEOMETRIC_REPRESENTATION_ITEM()
RATIONAL_B_SPLINE_SURFACE(((1.,0.707106781186548,1.,0.707106781186548,1.,
0.707106781186548,1.,0.707106781186548,1.),(0.707106781186533,0.499999999999989,
0.707106781186533,0.499999999999989,0.707106781186533,0.499999999999989,
0.707106781186533,0.499999999999989,0.707106781186533),(1.,0.707106781186548,
1.,0.707106781186548,1.,0.707106781186548,1.,0.707106781186548,1.)))
REPRESENTATION_ITEM('')
SURFACE()
);
#411=(
BOUNDED_SURFACE()
B_SPLINE_SURFACE(1,2,((#30592,#30593,#30594,#30595,#30596,#30597,#30598,
#30599,#30600,#30601,#30602,#30603,#30604,#30605,#30606,#30607,#30608,#30609,
#30610,#30611,#30612,#30613,#30614,#30615,#30616,#30617,#30618,#30619,#30620,
#30621,#30622,#30623,#30624,#30625,#30626,#30627,#30628,#30629,#30630,#30631,
#30632,#30633,#30634,#30635,#30636,#30637,#30638,#30639,#30640,#30641,#30642,
#30643,#30644,#30645,#30646,#30647,#30648,#30649,#30650,#30651,#30652,#30653,
#30654,#30655,#30656,#30657,#30658,#30659,#30660,#30661,#30662,#30663,#30664,
#30665,#30666,#30667,#30668,#30669,#30670,#30671,#30672,#30673,#30674,#30675,
#30676,#30677,#30678,#30679,#30680,#30681,#30682,#30683,#30684,#30685,#30686,
#30687,#30688,#30689,#30690,#30691,#30692,#30693,#30694,#30695,#30696,#30697,
#30698,#30699,#30700,#30701,#30702,#30703,#30704,#30705,#30706,#30707,#30708,
#30709,#30710,#30711,#30712,#30713,#30714,#30715,#30716,#30717,#30718,#30719,
#30720),(#30721,#30722,#30723,#30724,#30725,#30726,#30727,#30728,#30729,
#30730,#30731,#30732,#30733,#30734,#30735,#30736,#30737,#30738,#30739,#30740,
#30741,#30742,#30743,#30744,#30745,#30746,#30747,#30748,#30749,#30750,#30751,
#30752,#30753,#30754,#30755,#30756,#30757,#30758,#30759,#30760,#30761,#30762,
#30763,#30764,#30765,#30766,#30767,#30768,#30769,#30770,#30771,#30772,#30773,
#30774,#30775,#30776,#30777,#30778,#30779,#30780,#30781,#30782,#30783,#30784,
#30785,#30786,#30787,#30788,#30789,#30790,#30791,#30792,#30793,#30794,#30795,
#30796,#30797,#30798,#30799,#30800,#30801,#30802,#30803,#30804,#30805,#30806,
#30807,#30808,#30809,#30810,#30811,#30812,#30813,#30814,#30815,#30816,#30817,
#30818,#30819,#30820,#30821,#30822,#30823,#30824,#30825,#30826,#30827,#30828,
#30829,#30830,#30831,#30832,#30833,#30834,#30835,#30836,#30837,#30838,#30839,
#30840,#30841,#30842,#30843,#30844,#30845,#30846,#30847,#30848,#30849)),
 .UNSPECIFIED.,.F.,.F.,.F.)
B_SPLINE_SURFACE_WITH_KNOTS((2,2),(3,2,2,2,2,2,2,2,2,2,2,2,2,2,2,2,2,2,
2,2,2,2,2,2,2,2,2,2,2,2,2,2,2,2,2,2,2,2,2,2,2,2,2,2,2,2,2,2,2,2,2,2,2,2,
2,2,2,2,2,2,2,2,2,2,3),(-1.70594514575571E-6,1.),(0.,0.015625,0.03125,0.046875,
0.0625,0.078125,0.09375,0.109375,0.125,0.140625,0.15625,0.171875,0.1875,
0.203125,0.21875,0.234375,0.25,0.265625,0.28125,0.296875,0.3125,0.328125,
0.34375,0.359375,0.375,0.390625,0.40625,0.421875,0.4375,0.453125,0.46875,
0.484375,0.5,0.515625,0.53125,0.546875,0.5625,0.578125,0.59375,0.609375,
0.625,0.640625,0.65625,0.671875,0.6875,0.703125,0.71875,0.734375,0.75,0.765625,
0.78125,0.796875,0.8125,0.828125,0.84375,0.859375,0.875,0.890625,0.90625,
0.921875,0.9375,0.953125,0.96875,0.984375,1.),.UNSPECIFIED.)
GEOMETRIC_REPRESENTATION_ITEM()
RATIONAL_B_SPLINE_SURFACE(((1.,0.923879532511287,1.,0.923879532511287,1.,
0.923879532511287,1.,0.923879532511287,1.,0.923879532511287,1.,0.923879532511287,
1.,0.923879532511287,1.,0.923879532511287,1.,0.923879532511287,1.,0.923879532511287,
1.,0.923879532511287,1.,0.923879532511287,1.,0.923879532511287,1.,0.923879532511287,
1.,0.923879532511287,1.,0.923879532511287,1.,0.923879532511287,1.,0.923879532511287,
1.,0.923879532511287,1.,0.923879532511287,1.,0.923879532511287,1.,0.923879532511287,
1.,0.923879532511287,1.,0.923879532511287,1.,0.923879532511287,1.,0.923879532511287,
1.,0.923879532511287,1.,0.923879532511287,1.,0.923879532511287,1.,0.923879532511287,
1.,0.923879532511287,1.,0.923879532511287,1.,0.923879532511287,1.,0.923879532511287,
1.,0.923879532511287,1.,0.923879532511287,1.,0.923879532511287,1.,0.923879532511287,
1.,0.923879532511287,1.,0.923879532511287,1.,0.923879532511287,1.,0.923879532511287,
1.,0.923879532511287,1.,0.923879532511287,1.,0.923879532511287,1.,0.923879532511287,
1.,0.923879532511287,1.,0.923879532511287,1.,0.923879532511287,1.,0.923879532511287,
1.,0.923879532511287,1.,0.923879532511287,1.,0.923879532511287,1.,0.923879532511287,
1.,0.923879532511287,1.,0.923879532511287,1.,0.923879532511287,1.,0.923879532511287,
1.,0.923879532511287,1.,0.923879532511287,1.,0.923879532511287,1.,0.923879532511287,
1.,0.923879532511287,1.,0.923879532511287,1.),(1.,0.923879532511287,1.,
0.923879532511287,1.,0.923879532511287,1.,0.923879532511287,1.,0.923879532511287,
1.,0.923879532511287,1.,0.923879532511287,1.,0.923879532511287,1.,0.923879532511287,
1.,0.923879532511287,1.,0.923879532511287,1.,0.923879532511287,1.,0.923879532511287,
1.,0.923879532511287,1.,0.923879532511287,1.,0.923879532511287,1.,0.923879532511287,
1.,0.923879532511287,1.,0.923879532511287,1.,0.923879532511287,1.,0.923879532511287,
1.,0.923879532511287,1.,0.923879532511287,1.,0.923879532511287,1.,0.923879532511287,
1.,0.923879532511287,1.,0.923879532511287,1.,0.923879532511287,1.,0.923879532511287,
1.,0.923879532511287,1.,0.923879532511287,1.,0.923879532511287,1.,0.923879532511287,
1.,0.923879532511287,1.,0.923879532511287,1.,0.923879532511287,1.,0.923879532511287,
1.,0.923879532511287,1.,0.923879532511287,1.,0.923879532511287,1.,0.923879532511287,
1.,0.923879532511287,1.,0.923879532511287,1.,0.923879532511287,1.,0.923879532511287,
1.,0.923879532511287,1.,0.923879532511287,1.,0.923879532511287,1.,0.923879532511287,
1.,0.923879532511287,1.,0.923879532511287,1.,0.923879532511287,1.,0.923879532511287,
1.,0.923879532511287,1.,0.923879532511287,1.,0.923879532511287,1.,0.923879532511287,
1.,0.923879532511287,1.,0.923879532511287,1.,0.923879532511287,1.,0.923879532511287,
1.,0.923879532511287,1.,0.923879532511287,1.,0.923879532511287,1.)))
REPRESENTATION_ITEM('')
SURFACE()
);
#412=(
BOUNDED_SURFACE()
B_SPLINE_SURFACE(1,2,((#30903,#30904,#30905,#30906,#30907,#30908,#30909,
#30910,#30911,#30912,#30913,#30914,#30915,#30916,#30917,#30918,#30919,#30920,
#30921,#30922,#30923,#30924,#30925,#30926,#30927,#30928,#30929,#30930,#30931,
#30932,#30933,#30934,#30935,#30936,#30937,#30938,#30939,#30940,#30941,#30942,
#30943,#30944,#30945,#30946,#30947,#30948,#30949,#30950,#30951,#30952,#30953,
#30954,#30955,#30956,#30957,#30958,#30959,#30960,#30961,#30962,#30963,#30964,
#30965,#30966,#30967,#30968,#30969,#30970,#30971,#30972,#30973,#30974,#30975,
#30976,#30977,#30978,#30979,#30980,#30981,#30982,#30983,#30984,#30985,#30986,
#30987,#30988,#30989,#30990,#30991,#30992,#30993,#30994,#30995,#30996,#30997,
#30998,#30999,#31000,#31001,#31002,#31003,#31004,#31005,#31006,#31007,#31008,
#31009,#31010,#31011,#31012,#31013,#31014,#31015,#31016,#31017,#31018,#31019,
#31020,#31021,#31022,#31023,#31024,#31025,#31026,#31027,#31028,#31029,#31030,
#31031),(#31032,#31033,#31034,#31035,#31036,#31037,#31038,#31039,#31040,
#31041,#31042,#31043,#31044,#31045,#31046,#31047,#31048,#31049,#31050,#31051,
#31052,#31053,#31054,#31055,#31056,#31057,#31058,#31059,#31060,#31061,#31062,
#31063,#31064,#31065,#31066,#31067,#31068,#31069,#31070,#31071,#31072,#31073,
#31074,#31075,#31076,#31077,#31078,#31079,#31080,#31081,#31082,#31083,#31084,
#31085,#31086,#31087,#31088,#31089,#31090,#31091,#31092,#31093,#31094,#31095,
#31096,#31097,#31098,#31099,#31100,#31101,#31102,#31103,#31104,#31105,#31106,
#31107,#31108,#31109,#31110,#31111,#31112,#31113,#31114,#31115,#31116,#31117,
#31118,#31119,#31120,#31121,#31122,#31123,#31124,#31125,#31126,#31127,#31128,
#31129,#31130,#31131,#31132,#31133,#31134,#31135,#31136,#31137,#31138,#31139,
#31140,#31141,#31142,#31143,#31144,#31145,#31146,#31147,#31148,#31149,#31150,
#31151,#31152,#31153,#31154,#31155,#31156,#31157,#31158,#31159,#31160)),
 .UNSPECIFIED.,.F.,.F.,.F.)
B_SPLINE_SURFACE_WITH_KNOTS((2,2),(3,2,2,2,2,2,2,2,2,2,2,2,2,2,2,2,2,2,
2,2,2,2,2,2,2,2,2,2,2,2,2,2,2,2,2,2,2,2,2,2,2,2,2,2,2,2,2,2,2,2,2,2,2,2,
2,2,2,2,2,2,2,2,2,2,3),(0.,1.00002504461482),(0.,0.015625,0.03125,0.046875,
0.0625,0.078125,0.09375,0.109375,0.125,0.140625,0.15625,0.171875,0.1875,
0.203125,0.21875,0.234375,0.25,0.265625,0.28125,0.296875,0.3125,0.328125,
0.34375,0.359375,0.375,0.390625,0.40625,0.421875,0.4375,0.453125,0.46875,
0.484375,0.5,0.515625,0.53125,0.546875,0.5625,0.578125,0.59375,0.609375,
0.625,0.640625,0.65625,0.671875,0.6875,0.703125,0.71875,0.734375,0.75,0.765625,
0.78125,0.796875,0.8125,0.828125,0.84375,0.859375,0.875,0.890625,0.90625,
0.921875,0.9375,0.953125,0.96875,0.984375,1.),.UNSPECIFIED.)
GEOMETRIC_REPRESENTATION_ITEM()
RATIONAL_B_SPLINE_SURFACE(((1.,0.923879532511287,1.,0.923879532511287,1.,
0.923879532511287,1.,0.923879532511287,1.,0.923879532511287,1.,0.923879532511287,
1.,0.923879532511287,1.,0.923879532511287,1.,0.923879532511287,1.,0.923879532511287,
1.,0.923879532511287,1.,0.923879532511287,1.,0.923879532511287,1.,0.923879532511287,
1.,0.923879532511287,1.,0.923879532511287,1.,0.923879532511287,1.,0.923879532511287,
1.,0.923879532511287,1.,0.923879532511287,1.,0.923879532511287,1.,0.923879532511287,
1.,0.923879532511287,1.,0.923879532511287,1.,0.923879532511287,1.,0.923879532511287,
1.,0.923879532511287,1.,0.923879532511287,1.,0.923879532511287,1.,0.923879532511287,
1.,0.923879532511287,1.,0.923879532511287,1.,0.923879532511287,1.,0.923879532511287,
1.,0.923879532511287,1.,0.923879532511287,1.,0.923879532511287,1.,0.923879532511287,
1.,0.923879532511287,1.,0.923879532511287,1.,0.923879532511287,1.,0.923879532511287,
1.,0.923879532511287,1.,0.923879532511287,1.,0.923879532511287,1.,0.923879532511287,
1.,0.923879532511287,1.,0.923879532511287,1.,0.923879532511287,1.,0.923879532511287,
1.,0.923879532511287,1.,0.923879532511287,1.,0.923879532511287,1.,0.923879532511287,
1.,0.923879532511287,1.,0.923879532511287,1.,0.923879532511287,1.,0.923879532511287,
1.,0.923879532511287,1.,0.923879532511287,1.,0.923879532511287,1.,0.923879532511287,
1.,0.923879532511287,1.,0.923879532511287,1.),(1.,0.923879532511287,1.,
0.923879532511287,1.,0.923879532511287,1.,0.923879532511287,1.,0.923879532511287,
1.,0.923879532511287,1.,0.923879532511287,1.,0.923879532511287,1.,0.923879532511287,
1.,0.923879532511287,1.,0.923879532511287,1.,0.923879532511287,1.,0.923879532511287,
1.,0.923879532511287,1.,0.923879532511287,1.,0.923879532511287,1.,0.923879532511287,
1.,0.923879532511287,1.,0.923879532511287,1.,0.923879532511287,1.,0.923879532511287,
1.,0.923879532511287,1.,0.923879532511287,1.,0.923879532511287,1.,0.923879532511287,
1.,0.923879532511287,1.,0.923879532511287,1.,0.923879532511287,1.,0.923879532511287,
1.,0.923879532511287,1.,0.923879532511287,1.,0.923879532511287,1.,0.923879532511287,
1.,0.923879532511287,1.,0.923879532511287,1.,0.923879532511287,1.,0.923879532511287,
1.,0.923879532511287,1.,0.923879532511287,1.,0.923879532511287,1.,0.923879532511287,
1.,0.923879532511287,1.,0.923879532511287,1.,0.923879532511287,1.,0.923879532511287,
1.,0.923879532511287,1.,0.923879532511287,1.,0.923879532511287,1.,0.923879532511287,
1.,0.923879532511287,1.,0.923879532511287,1.,0.923879532511287,1.,0.923879532511287,
1.,0.923879532511287,1.,0.923879532511287,1.,0.923879532511287,1.,0.923879532511287,
1.,0.923879532511287,1.,0.923879532511287,1.,0.923879532511287,1.,0.923879532511287,
1.,0.923879532511287,1.,0.923879532511287,1.,0.923879532511287,1.)))
REPRESENTATION_ITEM('')
SURFACE()
);
#413=(
BOUNDED_SURFACE()
B_SPLINE_SURFACE(1,2,((#31853,#31854,#31855,#31856,#31857,#31858,#31859,
#31860,#31861,#31862,#31863,#31864,#31865,#31866,#31867,#31868,#31869,#31870,
#31871,#31872,#31873,#31874,#31875,#31876,#31877,#31878,#31879,#31880,#31881,
#31882,#31883,#31884,#31885,#31886,#31887,#31888,#31889,#31890,#31891,#31892,
#31893,#31894,#31895,#31896,#31897,#31898,#31899,#31900,#31901,#31902,#31903,
#31904,#31905,#31906,#31907,#31908,#31909,#31910,#31911,#31912,#31913,#31914,
#31915,#31916,#31917,#31918,#31919,#31920,#31921,#31922,#31923,#31924,#31925,
#31926,#31927,#31928,#31929,#31930,#31931,#31932,#31933,#31934,#31935,#31936,
#31937,#31938,#31939,#31940,#31941,#31942,#31943,#31944,#31945,#31946,#31947,
#31948,#31949,#31950,#31951,#31952,#31953,#31954,#31955,#31956,#31957,#31958,
#31959,#31960,#31961,#31962,#31963,#31964,#31965,#31966,#31967,#31968,#31969,
#31970,#31971,#31972,#31973,#31974,#31975,#31976,#31977,#31978,#31979,#31980,
#31981,#31982,#31983,#31984,#31985,#31986,#31987,#31988,#31989,#31990,#31991,
#31992,#31993,#31994,#31995,#31996,#31997,#31998,#31999,#32000,#32001,#32002,
#32003,#32004,#32005,#32006,#32007,#32008,#32009,#32010,#32011,#32012,#32013,
#32014,#32015,#32016,#32017,#32018,#32019,#32020,#32021,#32022,#32023,#32024,
#32025,#32026,#32027,#32028,#32029,#32030,#32031,#32032,#32033,#32034,#32035,
#32036,#32037,#32038,#32039,#32040,#32041,#32042,#32043,#32044,#32045,#32046,
#32047,#32048,#32049,#32050,#32051,#32052,#32053,#32054,#32055,#32056,#32057,
#32058,#32059,#32060,#32061,#32062,#32063,#32064,#32065,#32066,#32067,#32068,
#32069,#32070,#32071,#32072,#32073,#32074,#32075,#32076,#32077,#32078,#32079,
#32080,#32081,#32082,#32083,#32084,#32085,#32086,#32087,#32088,#32089,#32090,
#32091,#32092,#32093),(#32094,#32095,#32096,#32097,#32098,#32099,#32100,
#32101,#32102,#32103,#32104,#32105,#32106,#32107,#32108,#32109,#32110,#32111,
#32112,#32113,#32114,#32115,#32116,#32117,#32118,#32119,#32120,#32121,#32122,
#32123,#32124,#32125,#32126,#32127,#32128,#32129,#32130,#32131,#32132,#32133,
#32134,#32135,#32136,#32137,#32138,#32139,#32140,#32141,#32142,#32143,#32144,
#32145,#32146,#32147,#32148,#32149,#32150,#32151,#32152,#32153,#32154,#32155,
#32156,#32157,#32158,#32159,#32160,#32161,#32162,#32163,#32164,#32165,#32166,
#32167,#32168,#32169,#32170,#32171,#32172,#32173,#32174,#32175,#32176,#32177,
#32178,#32179,#32180,#32181,#32182,#32183,#32184,#32185,#32186,#32187,#32188,
#32189,#32190,#32191,#32192,#32193,#32194,#32195,#32196,#32197,#32198,#32199,
#32200,#32201,#32202,#32203,#32204,#32205,#32206,#32207,#32208,#32209,#32210,
#32211,#32212,#32213,#32214,#32215,#32216,#32217,#32218,#32219,#32220,#32221,
#32222,#32223,#32224,#32225,#32226,#32227,#32228,#32229,#32230,#32231,#32232,
#32233,#32234,#32235,#32236,#32237,#32238,#32239,#32240,#32241,#32242,#32243,
#32244,#32245,#32246,#32247,#32248,#32249,#32250,#32251,#32252,#32253,#32254,
#32255,#32256,#32257,#32258,#32259,#32260,#32261,#32262,#32263,#32264,#32265,
#32266,#32267,#32268,#32269,#32270,#32271,#32272,#32273,#32274,#32275,#32276,
#32277,#32278,#32279,#32280,#32281,#32282,#32283,#32284,#32285,#32286,#32287,
#32288,#32289,#32290,#32291,#32292,#32293,#32294,#32295,#32296,#32297,#32298,
#32299,#32300,#32301,#32302,#32303,#32304,#32305,#32306,#32307,#32308,#32309,
#32310,#32311,#32312,#32313,#32314,#32315,#32316,#32317,#32318,#32319,#32320,
#32321,#32322,#32323,#32324,#32325,#32326,#32327,#32328,#32329,#32330,#32331,
#32332,#32333,#32334)),.UNSPECIFIED.,.F.,.F.,.F.)
B_SPLINE_SURFACE_WITH_KNOTS((2,2),(3,2,2,2,2,2,2,2,2,2,2,2,2,2,2,2,2,2,
2,2,2,2,2,2,2,2,2,2,2,2,2,2,2,2,2,2,2,2,2,2,2,2,2,2,2,2,2,2,2,2,2,2,2,2,
2,2,2,2,2,2,2,2,2,2,2,2,2,2,2,2,2,2,2,2,2,2,2,2,2,2,2,2,2,2,2,2,2,2,2,2,
2,2,2,2,2,2,2,2,2,2,2,2,2,2,2,2,2,2,2,2,2,2,2,2,2,2,2,2,2,2,3),(0.,1.),
(0.,0.00833333333333333,0.0166666666666666,0.025,0.0333333333333333,0.0416666666666667,
0.05,0.0583333333333333,0.0666666666666667,0.075,0.0833333333333333,0.0916666666666667,
0.1,0.108333333333333,0.116666666666667,0.125,0.133333333333333,0.141666666666667,
0.15,0.158333333333333,0.166666666666667,0.175,0.183333333333334,0.191666666666667,
0.2,0.208333333333334,0.216666666666667,0.225,0.233333333333334,0.241666666666667,
0.25,0.258333333333334,0.266666666666666,0.275,0.283333333333334,0.291666666666667,
0.3,0.308333333333334,0.316666666666666,0.325,0.333333333333334,0.341666666666667,
0.35,0.358333333333334,0.366666666666666,0.375,0.383333333333334,0.391666666666666,
0.4,0.408333333333334,0.416666666666667,0.425,0.433333333333334,0.441666666666666,
0.45,0.458333333333333,0.466666666666667,0.475,0.483333333333333,0.491666666666667,
0.5,0.508333333333333,0.516666666666667,0.525,0.533333333333333,0.541666666666667,
0.55,0.558333333333333,0.566666666666667,0.575,0.583333333333333,0.591666666666667,
0.6,0.608333333333333,0.616666666666667,0.625,0.633333333333333,0.641666666666667,
0.65,0.658333333333333,0.666666666666667,0.675,0.683333333333333,0.691666666666667,
0.7,0.708333333333333,0.716666666666667,0.725,0.733333333333333,0.741666666666667,
0.75,0.758333333333333,0.766666666666667,0.775,0.783333333333333,0.791666666666667,
0.8,0.808333333333333,0.816666666666667,0.825,0.833333333333333,0.841666666666667,
0.85,0.858333333333333,0.866666666666667,0.875,0.883333333333333,0.891666666666667,
0.9,0.908333333333333,0.916666666666667,0.925,0.933333333333333,0.941666666666667,
0.95,0.958333333333333,0.966666666666667,0.975,0.983333333333333,0.991666666666667,
1.),.UNSPECIFIED.)
GEOMETRIC_REPRESENTATION_ITEM()
RATIONAL_B_SPLINE_SURFACE(((1.,0.866025403784439,1.,0.866025403784439,1.,
0.866025403784439,1.,0.866025403784439,1.,0.866025403784439,1.,0.866025403784439,
1.,0.866025403784439,1.,0.866025403784439,1.,0.866025403784439,1.,0.866025403784439,
1.,0.866025403784439,1.,0.866025403784439,1.,0.866025403784439,1.,0.866025403784439,
1.,0.866025403784439,1.,0.866025403784439,1.,0.866025403784439,1.,0.866025403784439,
1.,0.866025403784439,1.,0.866025403784439,1.,0.866025403784439,1.,0.866025403784439,
1.,0.866025403784439,1.,0.866025403784439,1.,0.866025403784439,1.,0.866025403784439,
1.,0.866025403784439,1.,0.866025403784439,1.,0.866025403784439,1.,0.866025403784439,
1.,0.866025403784439,1.,0.866025403784439,1.,0.866025403784439,1.,0.866025403784439,
1.,0.866025403784439,1.,0.866025403784439,1.,0.866025403784439,1.,0.866025403784439,
1.,0.866025403784439,1.,0.866025403784439,1.,0.866025403784439,1.,0.866025403784439,
1.,0.866025403784439,1.,0.866025403784439,1.,0.866025403784439,1.,0.866025403784439,
1.,0.866025403784439,1.,0.866025403784439,1.,0.866025403784439,1.,0.866025403784439,
1.,0.866025403784439,1.,0.866025403784439,1.,0.866025403784439,1.,0.866025403784439,
1.,0.866025403784439,1.,0.866025403784439,1.,0.866025403784439,1.,0.866025403784439,
1.,0.866025403784439,1.,0.866025403784439,1.,0.866025403784439,1.,0.866025403784439,
1.,0.866025403784439,1.,0.866025403784439,1.,0.866025403784439,1.,0.866025403784439,
1.,0.866025403784439,1.,0.866025403784439,1.,0.866025403784439,1.,0.866025403784439,
1.,0.866025403784439,1.,0.866025403784439,1.,0.866025403784439,1.,0.866025403784439,
1.,0.866025403784439,1.,0.866025403784439,1.,0.866025403784439,1.,0.866025403784439,
1.,0.866025403784439,1.,0.866025403784439,1.,0.866025403784439,1.,0.866025403784439,
1.,0.866025403784439,1.,0.866025403784439,1.,0.866025403784439,1.,0.866025403784439,
1.,0.866025403784439,1.,0.866025403784439,1.,0.866025403784439,1.,0.866025403784439,
1.,0.866025403784439,1.,0.866025403784439,1.,0.866025403784439,1.,0.866025403784439,
1.,0.866025403784439,1.,0.866025403784439,1.,0.866025403784439,1.,0.866025403784439,
1.,0.866025403784439,1.,0.866025403784439,1.,0.866025403784439,1.,0.866025403784439,
1.,0.866025403784439,1.,0.866025403784439,1.,0.866025403784439,1.,0.866025403784439,
1.,0.866025403784439,1.,0.866025403784439,1.,0.866025403784439,1.,0.866025403784439,
1.,0.866025403784439,1.,0.866025403784439,1.,0.866025403784439,1.,0.866025403784439,
1.,0.866025403784439,1.,0.866025403784439,1.,0.866025403784439,1.,0.866025403784439,
1.,0.866025403784439,1.,0.866025403784439,1.),(1.,0.866025403784439,1.,
0.866025403784439,1.,0.866025403784439,1.,0.866025403784439,1.,0.866025403784439,
1.,0.866025403784439,1.,0.866025403784439,1.,0.866025403784439,1.,0.866025403784439,
1.,0.866025403784439,1.,0.866025403784439,1.,0.866025403784439,1.,0.866025403784439,
1.,0.866025403784439,1.,0.866025403784439,1.,0.866025403784439,1.,0.866025403784439,
1.,0.866025403784439,1.,0.866025403784439,1.,0.866025403784439,1.,0.866025403784439,
1.,0.866025403784439,1.,0.866025403784439,1.,0.866025403784439,1.,0.866025403784439,
1.,0.866025403784439,1.,0.866025403784439,1.,0.866025403784439,1.,0.866025403784439,
1.,0.866025403784439,1.,0.866025403784439,1.,0.866025403784439,1.,0.866025403784439,
1.,0.866025403784439,1.,0.866025403784439,1.,0.866025403784439,1.,0.866025403784439,
1.,0.866025403784439,1.,0.866025403784439,1.,0.866025403784439,1.,0.866025403784439,
1.,0.866025403784439,1.,0.866025403784439,1.,0.866025403784439,1.,0.866025403784439,
1.,0.866025403784439,1.,0.866025403784439,1.,0.866025403784439,1.,0.866025403784439,
1.,0.866025403784439,1.,0.866025403784439,1.,0.866025403784439,1.,0.866025403784439,
1.,0.866025403784439,1.,0.866025403784439,1.,0.866025403784439,1.,0.866025403784439,
1.,0.866025403784439,1.,0.866025403784439,1.,0.866025403784439,1.,0.866025403784439,
1.,0.866025403784439,1.,0.866025403784439,1.,0.866025403784439,1.,0.866025403784439,
1.,0.866025403784439,1.,0.866025403784439,1.,0.866025403784439,1.,0.866025403784439,
1.,0.866025403784439,1.,0.866025403784439,1.,0.866025403784439,1.,0.866025403784439,
1.,0.866025403784439,1.,0.866025403784439,1.,0.866025403784439,1.,0.866025403784439,
1.,0.866025403784439,1.,0.866025403784439,1.,0.866025403784439,1.,0.866025403784439,
1.,0.866025403784439,1.,0.866025403784439,1.,0.866025403784439,1.,0.866025403784439,
1.,0.866025403784439,1.,0.866025403784439,1.,0.866025403784439,1.,0.866025403784439,
1.,0.866025403784439,1.,0.866025403784439,1.,0.866025403784439,1.,0.866025403784439,
1.,0.866025403784439,1.,0.866025403784439,1.,0.866025403784439,1.,0.866025403784439,
1.,0.866025403784439,1.,0.866025403784439,1.,0.866025403784439,1.,0.866025403784439,
1.,0.866025403784439,1.,0.866025403784439,1.,0.866025403784439,1.,0.866025403784439,
1.,0.866025403784439,1.,0.866025403784439,1.,0.866025403784439,1.,0.866025403784439,
1.,0.866025403784439,1.,0.866025403784439,1.,0.866025403784439,1.,0.866025403784439,
1.,0.866025403784439,1.,0.866025403784439,1.,0.866025403784439,1.,0.866025403784439,
1.,0.866025403784439,1.,0.866025403784439,1.,0.866025403784439,1.)))
REPRESENTATION_ITEM('')
SURFACE()
);
#414=(
BOUNDED_SURFACE()
B_SPLINE_SURFACE(1,2,((#32411,#32412,#32413,#32414,#32415,#32416,#32417,
#32418,#32419,#32420,#32421,#32422,#32423,#32424,#32425,#32426,#32427,#32428,
#32429,#32430,#32431,#32432,#32433,#32434,#32435,#32436,#32437,#32438,#32439,
#32440,#32441,#32442,#32443,#32444,#32445,#32446,#32447,#32448,#32449,#32450,
#32451,#32452,#32453,#32454,#32455,#32456,#32457,#32458,#32459,#32460,#32461,
#32462,#32463,#32464,#32465,#32466,#32467,#32468,#32469,#32470,#32471,#32472,
#32473,#32474,#32475,#32476,#32477,#32478,#32479,#32480,#32481,#32482,#32483,
#32484,#32485,#32486,#32487,#32488,#32489,#32490,#32491,#32492,#32493,#32494,
#32495,#32496,#32497,#32498,#32499,#32500,#32501,#32502,#32503,#32504,#32505,
#32506,#32507,#32508,#32509,#32510,#32511,#32512,#32513,#32514,#32515,#32516,
#32517,#32518,#32519,#32520,#32521,#32522,#32523,#32524,#32525,#32526,#32527,
#32528,#32529,#32530,#32531,#32532,#32533,#32534,#32535,#32536,#32537,#32538,
#32539,#32540,#32541,#32542,#32543,#32544,#32545,#32546,#32547,#32548,#32549,
#32550,#32551,#32552,#32553,#32554,#32555,#32556,#32557,#32558,#32559,#32560,
#32561,#32562,#32563,#32564,#32565,#32566,#32567,#32568,#32569,#32570,#32571,
#32572,#32573,#32574,#32575,#32576,#32577,#32578,#32579,#32580,#32581,#32582,
#32583,#32584,#32585,#32586,#32587,#32588,#32589,#32590,#32591,#32592,#32593,
#32594,#32595,#32596,#32597,#32598,#32599,#32600,#32601,#32602,#32603,#32604,
#32605,#32606,#32607,#32608,#32609,#32610,#32611,#32612,#32613,#32614,#32615,
#32616,#32617,#32618,#32619,#32620,#32621,#32622,#32623,#32624,#32625,#32626,
#32627,#32628,#32629,#32630,#32631,#32632,#32633,#32634,#32635,#32636,#32637,
#32638,#32639,#32640,#32641,#32642,#32643,#32644,#32645,#32646,#32647,#32648,
#32649,#32650,#32651),(#32652,#32653,#32654,#32655,#32656,#32657,#32658,
#32659,#32660,#32661,#32662,#32663,#32664,#32665,#32666,#32667,#32668,#32669,
#32670,#32671,#32672,#32673,#32674,#32675,#32676,#32677,#32678,#32679,#32680,
#32681,#32682,#32683,#32684,#32685,#32686,#32687,#32688,#32689,#32690,#32691,
#32692,#32693,#32694,#32695,#32696,#32697,#32698,#32699,#32700,#32701,#32702,
#32703,#32704,#32705,#32706,#32707,#32708,#32709,#32710,#32711,#32712,#32713,
#32714,#32715,#32716,#32717,#32718,#32719,#32720,#32721,#32722,#32723,#32724,
#32725,#32726,#32727,#32728,#32729,#32730,#32731,#32732,#32733,#32734,#32735,
#32736,#32737,#32738,#32739,#32740,#32741,#32742,#32743,#32744,#32745,#32746,
#32747,#32748,#32749,#32750,#32751,#32752,#32753,#32754,#32755,#32756,#32757,
#32758,#32759,#32760,#32761,#32762,#32763,#32764,#32765,#32766,#32767,#32768,
#32769,#32770,#32771,#32772,#32773,#32774,#32775,#32776,#32777,#32778,#32779,
#32780,#32781,#32782,#32783,#32784,#32785,#32786,#32787,#32788,#32789,#32790,
#32791,#32792,#32793,#32794,#32795,#32796,#32797,#32798,#32799,#32800,#32801,
#32802,#32803,#32804,#32805,#32806,#32807,#32808,#32809,#32810,#32811,#32812,
#32813,#32814,#32815,#32816,#32817,#32818,#32819,#32820,#32821,#32822,#32823,
#32824,#32825,#32826,#32827,#32828,#32829,#32830,#32831,#32832,#32833,#32834,
#32835,#32836,#32837,#32838,#32839,#32840,#32841,#32842,#32843,#32844,#32845,
#32846,#32847,#32848,#32849,#32850,#32851,#32852,#32853,#32854,#32855,#32856,
#32857,#32858,#32859,#32860,#32861,#32862,#32863,#32864,#32865,#32866,#32867,
#32868,#32869,#32870,#32871,#32872,#32873,#32874,#32875,#32876,#32877,#32878,
#32879,#32880,#32881,#32882,#32883,#32884,#32885,#32886,#32887,#32888,#32889,
#32890,#32891,#32892)),.UNSPECIFIED.,.F.,.F.,.F.)
B_SPLINE_SURFACE_WITH_KNOTS((2,2),(3,2,2,2,2,2,2,2,2,2,2,2,2,2,2,2,2,2,
2,2,2,2,2,2,2,2,2,2,2,2,2,2,2,2,2,2,2,2,2,2,2,2,2,2,2,2,2,2,2,2,2,2,2,2,
2,2,2,2,2,2,2,2,2,2,2,2,2,2,2,2,2,2,2,2,2,2,2,2,2,2,2,2,2,2,2,2,2,2,2,2,
2,2,2,2,2,2,2,2,2,2,2,2,2,2,2,2,2,2,2,2,2,2,2,2,2,2,2,2,2,2,3),(0.,1.),
(0.,0.00833333333333333,0.0166666666666666,0.025,0.0333333333333333,0.0416666666666667,
0.05,0.0583333333333333,0.0666666666666667,0.075,0.0833333333333333,0.0916666666666667,
0.1,0.108333333333333,0.116666666666667,0.125,0.133333333333333,0.141666666666667,
0.15,0.158333333333333,0.166666666666667,0.175,0.183333333333334,0.191666666666667,
0.2,0.208333333333334,0.216666666666667,0.225,0.233333333333334,0.241666666666667,
0.25,0.258333333333334,0.266666666666666,0.275,0.283333333333334,0.291666666666667,
0.3,0.308333333333334,0.316666666666666,0.325,0.333333333333334,0.341666666666667,
0.35,0.358333333333334,0.366666666666666,0.375,0.383333333333334,0.391666666666666,
0.4,0.408333333333334,0.416666666666667,0.425,0.433333333333334,0.441666666666666,
0.45,0.458333333333333,0.466666666666667,0.475,0.483333333333333,0.491666666666667,
0.5,0.508333333333333,0.516666666666667,0.525,0.533333333333333,0.541666666666667,
0.55,0.558333333333333,0.566666666666667,0.575,0.583333333333333,0.591666666666667,
0.6,0.608333333333333,0.616666666666667,0.625,0.633333333333333,0.641666666666667,
0.65,0.658333333333333,0.666666666666667,0.675,0.683333333333333,0.691666666666667,
0.7,0.708333333333333,0.716666666666667,0.725,0.733333333333333,0.741666666666667,
0.75,0.758333333333333,0.766666666666667,0.775,0.783333333333333,0.791666666666667,
0.8,0.808333333333333,0.816666666666667,0.825,0.833333333333333,0.841666666666667,
0.85,0.858333333333333,0.866666666666667,0.875,0.883333333333333,0.891666666666667,
0.9,0.908333333333333,0.916666666666667,0.925,0.933333333333333,0.941666666666667,
0.95,0.958333333333333,0.966666666666667,0.975,0.983333333333333,0.991666666666667,
1.),.UNSPECIFIED.)
GEOMETRIC_REPRESENTATION_ITEM()
RATIONAL_B_SPLINE_SURFACE(((1.,0.866025403784439,1.,0.866025403784439,1.,
0.866025403784439,1.,0.866025403784439,1.,0.866025403784439,1.,0.866025403784439,
1.,0.866025403784439,1.,0.866025403784439,1.,0.866025403784439,1.,0.866025403784439,
1.,0.866025403784439,1.,0.866025403784439,1.,0.866025403784439,1.,0.866025403784439,
1.,0.866025403784439,1.,0.866025403784439,1.,0.866025403784439,1.,0.866025403784439,
1.,0.866025403784439,1.,0.866025403784439,1.,0.866025403784439,1.,0.866025403784439,
1.,0.866025403784439,1.,0.866025403784439,1.,0.866025403784439,1.,0.866025403784439,
1.,0.866025403784439,1.,0.866025403784439,1.,0.866025403784439,1.,0.866025403784439,
1.,0.866025403784439,1.,0.866025403784439,1.,0.866025403784439,1.,0.866025403784439,
1.,0.866025403784439,1.,0.866025403784439,1.,0.866025403784439,1.,0.866025403784439,
1.,0.866025403784439,1.,0.866025403784439,1.,0.866025403784439,1.,0.866025403784439,
1.,0.866025403784439,1.,0.866025403784439,1.,0.866025403784439,1.,0.866025403784439,
1.,0.866025403784439,1.,0.866025403784439,1.,0.866025403784439,1.,0.866025403784439,
1.,0.866025403784439,1.,0.866025403784439,1.,0.866025403784439,1.,0.866025403784439,
1.,0.866025403784439,1.,0.866025403784439,1.,0.866025403784439,1.,0.866025403784439,
1.,0.866025403784439,1.,0.866025403784439,1.,0.866025403784439,1.,0.866025403784439,
1.,0.866025403784439,1.,0.866025403784439,1.,0.866025403784439,1.,0.866025403784439,
1.,0.866025403784439,1.,0.866025403784439,1.,0.866025403784439,1.,0.866025403784439,
1.,0.866025403784439,1.,0.866025403784439,1.,0.866025403784439,1.,0.866025403784439,
1.,0.866025403784439,1.,0.866025403784439,1.,0.866025403784439,1.,0.866025403784439,
1.,0.866025403784439,1.,0.866025403784439,1.,0.866025403784439,1.,0.866025403784439,
1.,0.866025403784439,1.,0.866025403784439,1.,0.866025403784439,1.,0.866025403784439,
1.,0.866025403784439,1.,0.866025403784439,1.,0.866025403784439,1.,0.866025403784439,
1.,0.866025403784439,1.,0.866025403784439,1.,0.866025403784439,1.,0.866025403784439,
1.,0.866025403784439,1.,0.866025403784439,1.,0.866025403784439,1.,0.866025403784439,
1.,0.866025403784439,1.,0.866025403784439,1.,0.866025403784439,1.,0.866025403784439,
1.,0.866025403784439,1.,0.866025403784439,1.,0.866025403784439,1.,0.866025403784439,
1.,0.866025403784439,1.,0.866025403784439,1.,0.866025403784439,1.,0.866025403784439,
1.,0.866025403784439,1.,0.866025403784439,1.,0.866025403784439,1.,0.866025403784439,
1.,0.866025403784439,1.,0.866025403784439,1.,0.866025403784439,1.,0.866025403784439,
1.,0.866025403784439,1.,0.866025403784439,1.),(1.,0.866025403784439,1.,
0.866025403784439,1.,0.866025403784439,1.,0.866025403784439,1.,0.866025403784439,
1.,0.866025403784439,1.,0.866025403784439,1.,0.866025403784439,1.,0.866025403784439,
1.,0.866025403784439,1.,0.866025403784439,1.,0.866025403784439,1.,0.866025403784439,
1.,0.866025403784439,1.,0.866025403784439,1.,0.866025403784439,1.,0.866025403784439,
1.,0.866025403784439,1.,0.866025403784439,1.,0.866025403784439,1.,0.866025403784439,
1.,0.866025403784439,1.,0.866025403784439,1.,0.866025403784439,1.,0.866025403784439,
1.,0.866025403784439,1.,0.866025403784439,1.,0.866025403784439,1.,0.866025403784439,
1.,0.866025403784439,1.,0.866025403784439,1.,0.866025403784439,1.,0.866025403784439,
1.,0.866025403784439,1.,0.866025403784439,1.,0.866025403784439,1.,0.866025403784439,
1.,0.866025403784439,1.,0.866025403784439,1.,0.866025403784439,1.,0.866025403784439,
1.,0.866025403784439,1.,0.866025403784439,1.,0.866025403784439,1.,0.866025403784439,
1.,0.866025403784439,1.,0.866025403784439,1.,0.866025403784439,1.,0.866025403784439,
1.,0.866025403784439,1.,0.866025403784439,1.,0.866025403784439,1.,0.866025403784439,
1.,0.866025403784439,1.,0.866025403784439,1.,0.866025403784439,1.,0.866025403784439,
1.,0.866025403784439,1.,0.866025403784439,1.,0.866025403784439,1.,0.866025403784439,
1.,0.866025403784439,1.,0.866025403784439,1.,0.866025403784439,1.,0.866025403784439,
1.,0.866025403784439,1.,0.866025403784439,1.,0.866025403784439,1.,0.866025403784439,
1.,0.866025403784439,1.,0.866025403784439,1.,0.866025403784439,1.,0.866025403784439,
1.,0.866025403784439,1.,0.866025403784439,1.,0.866025403784439,1.,0.866025403784439,
1.,0.866025403784439,1.,0.866025403784439,1.,0.866025403784439,1.,0.866025403784439,
1.,0.866025403784439,1.,0.866025403784439,1.,0.866025403784439,1.,0.866025403784439,
1.,0.866025403784439,1.,0.866025403784439,1.,0.866025403784439,1.,0.866025403784439,
1.,0.866025403784439,1.,0.866025403784439,1.,0.866025403784439,1.,0.866025403784439,
1.,0.866025403784439,1.,0.866025403784439,1.,0.866025403784439,1.,0.866025403784439,
1.,0.866025403784439,1.,0.866025403784439,1.,0.866025403784439,1.,0.866025403784439,
1.,0.866025403784439,1.,0.866025403784439,1.,0.866025403784439,1.,0.866025403784439,
1.,0.866025403784439,1.,0.866025403784439,1.,0.866025403784439,1.,0.866025403784439,
1.,0.866025403784439,1.,0.866025403784439,1.,0.866025403784439,1.,0.866025403784439,
1.,0.866025403784439,1.,0.866025403784439,1.,0.866025403784439,1.,0.866025403784439,
1.,0.866025403784439,1.,0.866025403784439,1.,0.866025403784439,1.)))
REPRESENTATION_ITEM('')
SURFACE()
);
#415=(
BOUNDED_SURFACE()
B_SPLINE_SURFACE(1,2,((#35210,#35211,#35212,#35213,#35214,#35215,#35216,
#35217,#35218,#35219,#35220,#35221,#35222,#35223,#35224,#35225,#35226,#35227,
#35228,#35229,#35230,#35231,#35232,#35233,#35234,#35235,#35236,#35237,#35238,
#35239,#35240,#35241,#35242,#35243,#35244,#35245,#35246,#35247,#35248,#35249,
#35250,#35251,#35252,#35253,#35254,#35255,#35256,#35257,#35258,#35259,#35260,
#35261,#35262,#35263,#35264,#35265,#35266,#35267,#35268,#35269,#35270,#35271,
#35272,#35273,#35274,#35275,#35276,#35277,#35278,#35279,#35280,#35281,#35282,
#35283,#35284,#35285,#35286,#35287,#35288,#35289,#35290,#35291,#35292,#35293,
#35294,#35295,#35296,#35297,#35298,#35299,#35300,#35301,#35302,#35303,#35304,
#35305,#35306,#35307,#35308,#35309,#35310,#35311,#35312,#35313,#35314,#35315,
#35316,#35317,#35318,#35319,#35320,#35321,#35322,#35323,#35324,#35325,#35326,
#35327,#35328,#35329,#35330,#35331,#35332,#35333,#35334,#35335,#35336,#35337,
#35338,#35339,#35340,#35341,#35342,#35343,#35344,#35345,#35346,#35347,#35348,
#35349,#35350,#35351,#35352,#35353,#35354,#35355,#35356,#35357,#35358,#35359,
#35360,#35361,#35362,#35363,#35364,#35365,#35366,#35367,#35368,#35369,#35370,
#35371,#35372,#35373,#35374,#35375,#35376,#35377,#35378),(#35379,#35380,
#35381,#35382,#35383,#35384,#35385,#35386,#35387,#35388,#35389,#35390,#35391,
#35392,#35393,#35394,#35395,#35396,#35397,#35398,#35399,#35400,#35401,#35402,
#35403,#35404,#35405,#35406,#35407,#35408,#35409,#35410,#35411,#35412,#35413,
#35414,#35415,#35416,#35417,#35418,#35419,#35420,#35421,#35422,#35423,#35424,
#35425,#35426,#35427,#35428,#35429,#35430,#35431,#35432,#35433,#35434,#35435,
#35436,#35437,#35438,#35439,#35440,#35441,#35442,#35443,#35444,#35445,#35446,
#35447,#35448,#35449,#35450,#35451,#35452,#35453,#35454,#35455,#35456,#35457,
#35458,#35459,#35460,#35461,#35462,#35463,#35464,#35465,#35466,#35467,#35468,
#35469,#35470,#35471,#35472,#35473,#35474,#35475,#35476,#35477,#35478,#35479,
#35480,#35481,#35482,#35483,#35484,#35485,#35486,#35487,#35488,#35489,#35490,
#35491,#35492,#35493,#35494,#35495,#35496,#35497,#35498,#35499,#35500,#35501,
#35502,#35503,#35504,#35505,#35506,#35507,#35508,#35509,#35510,#35511,#35512,
#35513,#35514,#35515,#35516,#35517,#35518,#35519,#35520,#35521,#35522,#35523,
#35524,#35525,#35526,#35527,#35528,#35529,#35530,#35531,#35532,#35533,#35534,
#35535,#35536,#35537,#35538,#35539,#35540,#35541,#35542,#35543,#35544,#35545,
#35546,#35547)),.UNSPECIFIED.,.F.,.F.,.F.)
B_SPLINE_SURFACE_WITH_KNOTS((2,2),(3,2,2,2,2,2,2,2,2,2,2,2,2,2,2,2,2,2,
2,2,2,2,2,2,2,2,2,2,2,2,2,2,2,2,2,2,2,2,2,2,2,2,2,2,2,2,2,2,2,2,2,2,2,2,
2,2,2,2,2,2,2,2,2,2,2,2,2,2,2,2,2,2,2,2,2,2,2,2,2,2,2,2,2,2,3),(0.,1.),
(0.,0.0119047619047619,0.0238095238095238,0.0357142857142857,0.0476190476190476,
0.0595238095238095,0.0714285714285714,0.0833333333333333,0.0952380952380952,
0.107142857142857,0.119047619047619,0.130952380952381,0.142857142857143,
0.154761904761905,0.166666666666667,0.178571428571428,0.19047619047619,
0.202380952380952,0.214285714285714,0.226190476190476,0.238095238095238,
0.25,0.261904761904762,0.273809523809524,0.285714285714286,0.297619047619048,
0.309523809523809,0.321428571428572,0.333333333333334,0.345238095238096,
0.357142857142857,0.369047619047619,0.380952380952381,0.392857142857143,
0.404761904761905,0.416666666666667,0.428571428571428,0.44047619047619,
0.452380952380952,0.464285714285714,0.476190476190476,0.488095238095238,
0.5,0.511904761904762,0.523809523809524,0.535714285714286,0.547619047619048,
0.55952380952381,0.571428571428571,0.583333333333333,0.595238095238095,
0.607142857142857,0.619047619047619,0.630952380952381,0.642857142857143,
0.654761904761905,0.666666666666667,0.678571428571429,0.690476190476191,
0.702380952380952,0.714285714285714,0.726190476190476,0.738095238095238,
0.75,0.761904761904762,0.773809523809524,0.785714285714286,0.797619047619048,
0.809523809523809,0.821428571428572,0.833333333333333,0.845238095238095,
0.857142857142857,0.869047619047619,0.880952380952381,0.892857142857143,
0.904761904761905,0.916666666666667,0.928571428571429,0.94047619047619,
0.952380952380952,0.964285714285714,0.976190476190476,0.988095238095238,
1.),.UNSPECIFIED.)
GEOMETRIC_REPRESENTATION_ITEM()
RATIONAL_B_SPLINE_SURFACE(((1.,0.866025403784439,1.,0.866025403784439,1.,
0.866025403784439,1.,0.866025403784439,1.,0.866025403784439,1.,0.866025403784439,
1.,0.866025403784439,1.,0.866025403784439,1.,0.866025403784439,1.,0.866025403784439,
1.,0.866025403784439,1.,0.866025403784439,1.,0.866025403784439,1.,0.866025403784439,
1.,0.866025403784439,1.,0.866025403784439,1.,0.866025403784439,1.,0.866025403784439,
1.,0.866025403784439,1.,0.866025403784439,1.,0.866025403784439,1.,0.866025403784439,
1.,0.866025403784439,1.,0.866025403784439,1.,0.866025403784439,1.,0.866025403784439,
1.,0.866025403784439,1.,0.866025403784439,1.,0.866025403784439,1.,0.866025403784439,
1.,0.866025403784439,1.,0.866025403784439,1.,0.866025403784439,1.,0.866025403784439,
1.,0.866025403784439,1.,0.866025403784439,1.,0.866025403784439,1.,0.866025403784439,
1.,0.866025403784439,1.,0.866025403784439,1.,0.866025403784439,1.,0.866025403784439,
1.,0.866025403784439,1.,0.866025403784439,1.,0.866025403784439,1.,0.866025403784439,
1.,0.866025403784439,1.,0.866025403784439,1.,0.866025403784439,1.,0.866025403784439,
1.,0.866025403784439,1.,0.866025403784439,1.,0.866025403784439,1.,0.866025403784439,
1.,0.866025403784439,1.,0.866025403784439,1.,0.866025403784439,1.,0.866025403784439,
1.,0.866025403784439,1.,0.866025403784439,1.,0.866025403784439,1.,0.866025403784439,
1.,0.866025403784439,1.,0.866025403784439,1.,0.866025403784439,1.,0.866025403784439,
1.,0.866025403784439,1.,0.866025403784439,1.,0.866025403784439,1.,0.866025403784439,
1.,0.866025403784439,1.,0.866025403784439,1.,0.866025403784439,1.,0.866025403784439,
1.,0.866025403784439,1.,0.866025403784439,1.,0.866025403784439,1.,0.866025403784439,
1.,0.866025403784439,1.,0.866025403784439,1.,0.866025403784439,1.,0.866025403784439,
1.,0.866025403784439,1.,0.866025403784439,1.),(1.,0.866025403784439,1.,
0.866025403784439,1.,0.866025403784439,1.,0.866025403784439,1.,0.866025403784439,
1.,0.866025403784439,1.,0.866025403784439,1.,0.866025403784439,1.,0.866025403784439,
1.,0.866025403784439,1.,0.866025403784439,1.,0.866025403784439,1.,0.866025403784439,
1.,0.866025403784439,1.,0.866025403784439,1.,0.866025403784439,1.,0.866025403784439,
1.,0.866025403784439,1.,0.866025403784439,1.,0.866025403784439,1.,0.866025403784439,
1.,0.866025403784439,1.,0.866025403784439,1.,0.866025403784439,1.,0.866025403784439,
1.,0.866025403784439,1.,0.866025403784439,1.,0.866025403784439,1.,0.866025403784439,
1.,0.866025403784439,1.,0.866025403784439,1.,0.866025403784439,1.,0.866025403784439,
1.,0.866025403784439,1.,0.866025403784439,1.,0.866025403784439,1.,0.866025403784439,
1.,0.866025403784439,1.,0.866025403784439,1.,0.866025403784439,1.,0.866025403784439,
1.,0.866025403784439,1.,0.866025403784439,1.,0.866025403784439,1.,0.866025403784439,
1.,0.866025403784439,1.,0.866025403784439,1.,0.866025403784439,1.,0.866025403784439,
1.,0.866025403784439,1.,0.866025403784439,1.,0.866025403784439,1.,0.866025403784439,
1.,0.866025403784439,1.,0.866025403784439,1.,0.866025403784439,1.,0.866025403784439,
1.,0.866025403784439,1.,0.866025403784439,1.,0.866025403784439,1.,0.866025403784439,
1.,0.866025403784439,1.,0.866025403784439,1.,0.866025403784439,1.,0.866025403784439,
1.,0.866025403784439,1.,0.866025403784439,1.,0.866025403784439,1.,0.866025403784439,
1.,0.866025403784439,1.,0.866025403784439,1.,0.866025403784439,1.,0.866025403784439,
1.,0.866025403784439,1.,0.866025403784439,1.,0.866025403784439,1.,0.866025403784439,
1.,0.866025403784439,1.,0.866025403784439,1.,0.866025403784439,1.,0.866025403784439,
1.,0.866025403784439,1.,0.866025403784439,1.,0.866025403784439,1.)))
REPRESENTATION_ITEM('')
SURFACE()
);
#416=(
BOUNDED_SURFACE()
B_SPLINE_SURFACE(1,2,((#35613,#35614,#35615,#35616,#35617,#35618,#35619,
#35620,#35621,#35622,#35623,#35624,#35625,#35626,#35627,#35628,#35629,#35630,
#35631,#35632,#35633,#35634,#35635,#35636,#35637,#35638,#35639,#35640,#35641,
#35642,#35643,#35644,#35645,#35646,#35647,#35648,#35649,#35650,#35651,#35652,
#35653,#35654,#35655,#35656,#35657,#35658,#35659,#35660,#35661,#35662,#35663,
#35664,#35665,#35666,#35667,#35668,#35669,#35670,#35671,#35672,#35673,#35674,
#35675,#35676,#35677,#35678,#35679,#35680,#35681,#35682,#35683,#35684,#35685,
#35686,#35687,#35688,#35689,#35690,#35691,#35692,#35693,#35694,#35695,#35696,
#35697,#35698,#35699,#35700,#35701,#35702,#35703,#35704,#35705,#35706,#35707,
#35708,#35709,#35710,#35711,#35712,#35713,#35714,#35715,#35716,#35717,#35718,
#35719,#35720,#35721,#35722,#35723,#35724,#35725,#35726,#35727,#35728,#35729,
#35730,#35731,#35732,#35733,#35734,#35735,#35736,#35737,#35738,#35739,#35740,
#35741,#35742,#35743,#35744,#35745,#35746,#35747,#35748,#35749,#35750,#35751,
#35752,#35753,#35754,#35755,#35756,#35757,#35758,#35759,#35760,#35761,#35762,
#35763,#35764,#35765,#35766,#35767,#35768,#35769,#35770,#35771,#35772,#35773,
#35774,#35775,#35776,#35777,#35778,#35779,#35780,#35781),(#35782,#35783,
#35784,#35785,#35786,#35787,#35788,#35789,#35790,#35791,#35792,#35793,#35794,
#35795,#35796,#35797,#35798,#35799,#35800,#35801,#35802,#35803,#35804,#35805,
#35806,#35807,#35808,#35809,#35810,#35811,#35812,#35813,#35814,#35815,#35816,
#35817,#35818,#35819,#35820,#35821,#35822,#35823,#35824,#35825,#35826,#35827,
#35828,#35829,#35830,#35831,#35832,#35833,#35834,#35835,#35836,#35837,#35838,
#35839,#35840,#35841,#35842,#35843,#35844,#35845,#35846,#35847,#35848,#35849,
#35850,#35851,#35852,#35853,#35854,#35855,#35856,#35857,#35858,#35859,#35860,
#35861,#35862,#35863,#35864,#35865,#35866,#35867,#35868,#35869,#35870,#35871,
#35872,#35873,#35874,#35875,#35876,#35877,#35878,#35879,#35880,#35881,#35882,
#35883,#35884,#35885,#35886,#35887,#35888,#35889,#35890,#35891,#35892,#35893,
#35894,#35895,#35896,#35897,#35898,#35899,#35900,#35901,#35902,#35903,#35904,
#35905,#35906,#35907,#35908,#35909,#35910,#35911,#35912,#35913,#35914,#35915,
#35916,#35917,#35918,#35919,#35920,#35921,#35922,#35923,#35924,#35925,#35926,
#35927,#35928,#35929,#35930,#35931,#35932,#35933,#35934,#35935,#35936,#35937,
#35938,#35939,#35940,#35941,#35942,#35943,#35944,#35945,#35946,#35947,#35948,
#35949,#35950)),.UNSPECIFIED.,.F.,.F.,.F.)
B_SPLINE_SURFACE_WITH_KNOTS((2,2),(3,2,2,2,2,2,2,2,2,2,2,2,2,2,2,2,2,2,
2,2,2,2,2,2,2,2,2,2,2,2,2,2,2,2,2,2,2,2,2,2,2,2,2,2,2,2,2,2,2,2,2,2,2,2,
2,2,2,2,2,2,2,2,2,2,2,2,2,2,2,2,2,2,2,2,2,2,2,2,2,2,2,2,2,2,3),(0.,1.),
(0.,0.0119047619047619,0.0238095238095238,0.0357142857142857,0.0476190476190476,
0.0595238095238095,0.0714285714285714,0.0833333333333333,0.0952380952380952,
0.107142857142857,0.119047619047619,0.130952380952381,0.142857142857143,
0.154761904761905,0.166666666666667,0.178571428571428,0.19047619047619,
0.202380952380952,0.214285714285714,0.226190476190476,0.238095238095238,
0.25,0.261904761904762,0.273809523809524,0.285714285714286,0.297619047619048,
0.309523809523809,0.321428571428572,0.333333333333334,0.345238095238096,
0.357142857142857,0.369047619047619,0.380952380952381,0.392857142857143,
0.404761904761905,0.416666666666667,0.428571428571428,0.44047619047619,
0.452380952380952,0.464285714285714,0.476190476190476,0.488095238095238,
0.5,0.511904761904762,0.523809523809524,0.535714285714286,0.547619047619048,
0.55952380952381,0.571428571428571,0.583333333333333,0.595238095238095,
0.607142857142857,0.619047619047619,0.630952380952381,0.642857142857143,
0.654761904761905,0.666666666666667,0.678571428571429,0.690476190476191,
0.702380952380952,0.714285714285714,0.726190476190476,0.738095238095238,
0.75,0.761904761904762,0.773809523809524,0.785714285714286,0.797619047619048,
0.809523809523809,0.821428571428572,0.833333333333333,0.845238095238095,
0.857142857142857,0.869047619047619,0.880952380952381,0.892857142857143,
0.904761904761905,0.916666666666667,0.928571428571429,0.94047619047619,
0.952380952380952,0.964285714285714,0.976190476190476,0.988095238095238,
1.),.UNSPECIFIED.)
GEOMETRIC_REPRESENTATION_ITEM()
RATIONAL_B_SPLINE_SURFACE(((1.,0.866025403784439,1.,0.866025403784439,1.,
0.866025403784439,1.,0.866025403784439,1.,0.866025403784439,1.,0.866025403784439,
1.,0.866025403784439,1.,0.866025403784439,1.,0.866025403784439,1.,0.866025403784439,
1.,0.866025403784439,1.,0.866025403784439,1.,0.866025403784439,1.,0.866025403784439,
1.,0.866025403784439,1.,0.866025403784439,1.,0.866025403784439,1.,0.866025403784439,
1.,0.866025403784439,1.,0.866025403784439,1.,0.866025403784439,1.,0.866025403784439,
1.,0.866025403784439,1.,0.866025403784439,1.,0.866025403784439,1.,0.866025403784439,
1.,0.866025403784439,1.,0.866025403784439,1.,0.866025403784439,1.,0.866025403784439,
1.,0.866025403784439,1.,0.866025403784439,1.,0.866025403784439,1.,0.866025403784439,
1.,0.866025403784439,1.,0.866025403784439,1.,0.866025403784439,1.,0.866025403784439,
1.,0.866025403784439,1.,0.866025403784439,1.,0.866025403784439,1.,0.866025403784439,
1.,0.866025403784439,1.,0.866025403784439,1.,0.866025403784439,1.,0.866025403784439,
1.,0.866025403784439,1.,0.866025403784439,1.,0.866025403784439,1.,0.866025403784439,
1.,0.866025403784439,1.,0.866025403784439,1.,0.866025403784439,1.,0.866025403784439,
1.,0.866025403784439,1.,0.866025403784439,1.,0.866025403784439,1.,0.866025403784439,
1.,0.866025403784439,1.,0.866025403784439,1.,0.866025403784439,1.,0.866025403784439,
1.,0.866025403784439,1.,0.866025403784439,1.,0.866025403784439,1.,0.866025403784439,
1.,0.866025403784439,1.,0.866025403784439,1.,0.866025403784439,1.,0.866025403784439,
1.,0.866025403784439,1.,0.866025403784439,1.,0.866025403784439,1.,0.866025403784439,
1.,0.866025403784439,1.,0.866025403784439,1.,0.866025403784439,1.,0.866025403784439,
1.,0.866025403784439,1.,0.866025403784439,1.,0.866025403784439,1.,0.866025403784439,
1.,0.866025403784439,1.,0.866025403784439,1.),(1.,0.866025403784439,1.,
0.866025403784439,1.,0.866025403784439,1.,0.866025403784439,1.,0.866025403784439,
1.,0.866025403784439,1.,0.866025403784439,1.,0.866025403784439,1.,0.866025403784439,
1.,0.866025403784439,1.,0.866025403784439,1.,0.866025403784439,1.,0.866025403784439,
1.,0.866025403784439,1.,0.866025403784439,1.,0.866025403784439,1.,0.866025403784439,
1.,0.866025403784439,1.,0.866025403784439,1.,0.866025403784439,1.,0.866025403784439,
1.,0.866025403784439,1.,0.866025403784439,1.,0.866025403784439,1.,0.866025403784439,
1.,0.866025403784439,1.,0.866025403784439,1.,0.866025403784439,1.,0.866025403784439,
1.,0.866025403784439,1.,0.866025403784439,1.,0.866025403784439,1.,0.866025403784439,
1.,0.866025403784439,1.,0.866025403784439,1.,0.866025403784439,1.,0.866025403784439,
1.,0.866025403784439,1.,0.866025403784439,1.,0.866025403784439,1.,0.866025403784439,
1.,0.866025403784439,1.,0.866025403784439,1.,0.866025403784439,1.,0.866025403784439,
1.,0.866025403784439,1.,0.866025403784439,1.,0.866025403784439,1.,0.866025403784439,
1.,0.866025403784439,1.,0.866025403784439,1.,0.866025403784439,1.,0.866025403784439,
1.,0.866025403784439,1.,0.866025403784439,1.,0.866025403784439,1.,0.866025403784439,
1.,0.866025403784439,1.,0.866025403784439,1.,0.866025403784439,1.,0.866025403784439,
1.,0.866025403784439,1.,0.866025403784439,1.,0.866025403784439,1.,0.866025403784439,
1.,0.866025403784439,1.,0.866025403784439,1.,0.866025403784439,1.,0.866025403784439,
1.,0.866025403784439,1.,0.866025403784439,1.,0.866025403784439,1.,0.866025403784439,
1.,0.866025403784439,1.,0.866025403784439,1.,0.866025403784439,1.,0.866025403784439,
1.,0.866025403784439,1.,0.866025403784439,1.,0.866025403784439,1.,0.866025403784439,
1.,0.866025403784439,1.,0.866025403784439,1.,0.866025403784439,1.)))
REPRESENTATION_ITEM('')
SURFACE()
);
#417=ELLIPSE('',#18107,0.707106781183618,0.499999999997816);
#418=ELLIPSE('',#18108,0.70710678118541,0.499999999999275);
#419=ELLIPSE('',#18109,0.707106781187129,0.500000000000412);
#420=ELLIPSE('',#18110,0.707106781186662,0.500000000000074);
#421=ELLIPSE('',#18114,0.707106781185328,0.499999999999127);
#422=ELLIPSE('',#18115,0.707106781186805,0.500000000000239);
#423=ELLIPSE('',#18116,0.707106781186168,0.499999999999746);
#424=ELLIPSE('',#18117,0.707106781186428,0.499999999999895);
#425=ELLIPSE('',#18121,0.707106781186371,0.500000000000029);
#426=ELLIPSE('',#18122,0.707106781185591,0.499999999999375);
#427=ELLIPSE('',#18123,0.707106781187582,0.500000000000786);
#428=ELLIPSE('',#18124,0.707106781187168,0.500000000000398);
#429=ELLIPSE('',#18811,1.60424783344755,1.60000000000667);
#430=ELLIPSE('',#19087,1.9066404831829,1.40000000000002);
#431=ELLIPSE('',#19093,1.9066404831826,1.40000000000005);
#432=ELLIPSE('',#19299,0.715693849834519,0.699999999997075);
#433=ELLIPSE('',#19300,0.715693849836967,0.699999999999567);
#434=ELLIPSE('',#19301,0.720792014405194,0.700000000003498);
#435=ELLIPSE('',#19302,0.720792014401284,0.699999999999729);
#436=ELLIPSE('',#19304,0.704512458806093,0.699999999997662);
#437=ELLIPSE('',#19305,0.70237579871988,0.699999999997508);
#438=ELLIPSE('',#19306,0.702375798725131,0.700000000002555);
#439=ELLIPSE('',#19307,0.704512458813107,0.700000000004563);
#440=ELLIPSE('',#19309,0.624754966914843,0.599999999999018);
#441=ELLIPSE('',#19310,0.624754966916465,0.600000000000533);
#442=ELLIPSE('',#19311,0.624754966913492,0.599999999997754);
#443=ELLIPSE('',#19312,0.624754966919923,0.600000000003613);
#444=ELLIPSE('',#19339,0.577350269188758,0.49999999999938);
#445=ELLIPSE('',#19340,0.577350269187932,0.499999999998527);
#446=ELLIPSE('',#19342,0.577350269187005,0.499999999997962);
#447=ELLIPSE('',#19344,0.577350269188423,0.499999999999111);
#448=ELLIPSE('',#19346,0.577350269189091,0.499999999999555);
#449=ELLIPSE('',#19348,0.577350269191436,0.500000000001306);
#450=SHAPE_REPRESENTATION_RELATIONSHIP('SRR','None',#36706,#460);
#451=SHAPE_REPRESENTATION_RELATIONSHIP('SRR','None',#36707,#461);
#452=SHAPE_REPRESENTATION_RELATIONSHIP('SRR','None',#36708,#462);
#453=SHAPE_REPRESENTATION_RELATIONSHIP('SRR','None',#36709,#463);
#454=SHAPE_REPRESENTATION_RELATIONSHIP('SRR','None',#36710,#464);
#455=SHAPE_REPRESENTATION_RELATIONSHIP('SRR','None',#36711,#465);
#456=SHAPE_REPRESENTATION_RELATIONSHIP('SRR','None',#36712,#466);
#457=SHAPE_REPRESENTATION_RELATIONSHIP('SRR','None',#36713,#467);
#458=SHAPE_REPRESENTATION_RELATIONSHIP('SRR','None',#36714,#468);
#459=SHAPE_REPRESENTATION_RELATIONSHIP('SRR','None',#36715,#469);
#460=ADVANCED_BREP_SHAPE_REPRESENTATION('',(#480),#36658);
#461=ADVANCED_BREP_SHAPE_REPRESENTATION('',(#481),#36659);
#462=ADVANCED_BREP_SHAPE_REPRESENTATION('',(#482),#36660);
#463=ADVANCED_BREP_SHAPE_REPRESENTATION('',(#483),#36661);
#464=ADVANCED_BREP_SHAPE_REPRESENTATION('',(#484),#36662);
#465=ADVANCED_BREP_SHAPE_REPRESENTATION('',(#485),#36663);
#466=ADVANCED_BREP_SHAPE_REPRESENTATION('',(#486),#36664);
#467=ADVANCED_BREP_SHAPE_REPRESENTATION('',(#487),#36665);
#468=ADVANCED_BREP_SHAPE_REPRESENTATION('',(#52),#36666);
#469=ADVANCED_BREP_SHAPE_REPRESENTATION('',(#488),#36667);
#470=STYLED_ITEM('',(#36765),#480);
#471=STYLED_ITEM('',(#36766),#481);
#472=STYLED_ITEM('',(#36767),#482);
#473=STYLED_ITEM('',(#36768),#483);
#474=STYLED_ITEM('',(#36769),#484);
#475=STYLED_ITEM('',(#36770),#485);
#476=STYLED_ITEM('',(#36765),#486);
#477=STYLED_ITEM('',(#36769),#487);
#478=STYLED_ITEM('',(#36770),#52);
#479=STYLED_ITEM('',(#36766),#488);
#480=MANIFOLD_SOLID_BREP('Body1',#17793);
#481=MANIFOLD_SOLID_BREP('Body1',#17794);
#482=MANIFOLD_SOLID_BREP('Body1',#17795);
#483=MANIFOLD_SOLID_BREP('Body1',#17796);
#484=MANIFOLD_SOLID_BREP('Body1',#17797);
#485=MANIFOLD_SOLID_BREP('Body1',#17798);
#486=MANIFOLD_SOLID_BREP('Body1',#17799);
#487=MANIFOLD_SOLID_BREP('Body1',#17800);
#488=MANIFOLD_SOLID_BREP('Body1',#17803);
#489=CYLINDRICAL_SURFACE('',#17972,0.750000000000001);
#490=CYLINDRICAL_SURFACE('',#17973,0.750000000000001);
#491=CYLINDRICAL_SURFACE('',#17974,0.75);
#492=CYLINDRICAL_SURFACE('',#17975,0.75);
#493=CYLINDRICAL_SURFACE('',#17976,0.75);
#494=CYLINDRICAL_SURFACE('',#17977,0.75);
#495=CYLINDRICAL_SURFACE('',#17978,0.750000000000001);
#496=CYLINDRICAL_SURFACE('',#17979,0.750000000000001);
#497=CYLINDRICAL_SURFACE('',#17980,0.750000000000001);
#498=CYLINDRICAL_SURFACE('',#17981,0.750000000000001);
#499=CYLINDRICAL_SURFACE('',#17982,0.750000000000001);
#500=CYLINDRICAL_SURFACE('',#17983,0.750000000000001);
#501=CYLINDRICAL_SURFACE('',#17984,0.750000000000001);
#502=CYLINDRICAL_SURFACE('',#17985,0.750000000000001);
#503=CYLINDRICAL_SURFACE('',#17986,0.750000000000001);
#504=CYLINDRICAL_SURFACE('',#17987,0.750000000000001);
#505=CYLINDRICAL_SURFACE('',#17988,0.750000000000001);
#506=CYLINDRICAL_SURFACE('',#17989,0.750000000000001);
#507=CYLINDRICAL_SURFACE('',#17990,0.750000000000001);
#508=CYLINDRICAL_SURFACE('',#17991,0.750000000000001);
#509=CYLINDRICAL_SURFACE('',#17992,0.750000000000001);
#510=CYLINDRICAL_SURFACE('',#17993,0.750000000000001);
#511=CYLINDRICAL_SURFACE('',#17994,0.750000000000001);
#512=CYLINDRICAL_SURFACE('',#17995,0.750000000000001);
#513=CYLINDRICAL_SURFACE('',#17996,0.750000000000001);
#514=CYLINDRICAL_SURFACE('',#17997,0.750000000000001);
#515=CYLINDRICAL_SURFACE('',#18106,0.5);
#516=CYLINDRICAL_SURFACE('',#18111,0.5);
#517=CYLINDRICAL_SURFACE('',#18112,0.5);
#518=CYLINDRICAL_SURFACE('',#18113,0.5);
#519=CYLINDRICAL_SURFACE('',#18118,0.5);
#520=CYLINDRICAL_SURFACE('',#18119,0.5);
#521=CYLINDRICAL_SURFACE('',#18120,0.5);
#522=CYLINDRICAL_SURFACE('',#18125,0.5);
#523=CYLINDRICAL_SURFACE('',#18126,0.5);
#524=CYLINDRICAL_SURFACE('',#18131,0.5);
#525=CYLINDRICAL_SURFACE('',#18136,0.5);
#526=CYLINDRICAL_SURFACE('',#18140,0.5);
#527=CYLINDRICAL_SURFACE('',#18147,0.5);
#528=CYLINDRICAL_SURFACE('',#18157,0.5);
#529=CYLINDRICAL_SURFACE('',#18160,0.5);
#530=CYLINDRICAL_SURFACE('',#18167,0.5);
#531=CYLINDRICAL_SURFACE('',#18170,0.5);
#532=CYLINDRICAL_SURFACE('',#18173,0.5);
#533=CYLINDRICAL_SURFACE('',#18176,0.5);
#534=CYLINDRICAL_SURFACE('',#18197,0.5);
#535=CYLINDRICAL_SURFACE('',#18200,0.5);
#536=CYLINDRICAL_SURFACE('',#18203,0.5);
#537=CYLINDRICAL_SURFACE('',#18206,0.5);
#538=CYLINDRICAL_SURFACE('',#18209,1.);
#539=CYLINDRICAL_SURFACE('',#18231,1.6);
#540=CYLINDRICAL_SURFACE('',#18235,1.6);
#541=CYLINDRICAL_SURFACE('',#18239,1.6);
#542=CYLINDRICAL_SURFACE('',#18243,1.6);
#543=CYLINDRICAL_SURFACE('',#18253,2.15235845279182);
#544=CYLINDRICAL_SURFACE('',#18258,1.76114216495771);
#545=CYLINDRICAL_SURFACE('',#18261,1.76114216495771);
#546=CYLINDRICAL_SURFACE('',#18262,1.76114216495771);
#547=CYLINDRICAL_SURFACE('',#18350,31.5);
#548=CYLINDRICAL_SURFACE('',#18351,17.9);
#549=CYLINDRICAL_SURFACE('',#18372,15.8);
#550=CYLINDRICAL_SURFACE('',#18374,10.2);
#551=CYLINDRICAL_SURFACE('',#18377,12.5);
#552=CYLINDRICAL_SURFACE('',#18394,0.250000000000003);
#553=CYLINDRICAL_SURFACE('',#18402,0.249999569584526);
#554=CYLINDRICAL_SURFACE('',#18403,0.249999999999998);
#555=CYLINDRICAL_SURFACE('',#18417,0.250000000000003);
#556=CYLINDRICAL_SURFACE('',#18418,0.249999570396522);
#557=CYLINDRICAL_SURFACE('',#18419,0.249999576130625);
#558=CYLINDRICAL_SURFACE('',#18420,0.249999999999998);
#559=CYLINDRICAL_SURFACE('',#18423,0.249999999999998);
#560=CYLINDRICAL_SURFACE('',#18434,0.249999575380867);
#561=CYLINDRICAL_SURFACE('',#18438,0.250000000000003);
#562=CYLINDRICAL_SURFACE('',#18442,0.249999999999998);
#563=CYLINDRICAL_SURFACE('',#18451,0.250000000000003);
#564=CYLINDRICAL_SURFACE('',#18454,0.249999569575431);
#565=CYLINDRICAL_SURFACE('',#18455,0.249999999999998);
#566=CYLINDRICAL_SURFACE('',#18456,0.249999999999998);
#567=CYLINDRICAL_SURFACE('',#18471,0.250000000000006);
#568=CYLINDRICAL_SURFACE('',#18472,0.249999566833149);
#569=CYLINDRICAL_SURFACE('',#18473,0.24999957614651);
#570=CYLINDRICAL_SURFACE('',#18475,0.249999999999998);
#571=CYLINDRICAL_SURFACE('',#18477,0.249999999999996);
#572=CYLINDRICAL_SURFACE('',#18488,0.249999578947113);
#573=CYLINDRICAL_SURFACE('',#18492,0.249999999999998);
#574=CYLINDRICAL_SURFACE('',#18497,0.249999999999996);
#575=CYLINDRICAL_SURFACE('',#18505,0.250000000000006);
#576=CYLINDRICAL_SURFACE('',#18509,0.249999575366884);
#577=CYLINDRICAL_SURFACE('',#18510,0.250000000000004);
#578=CYLINDRICAL_SURFACE('',#18511,0.250000000000004);
#579=CYLINDRICAL_SURFACE('',#18526,0.250000000000004);
#580=CYLINDRICAL_SURFACE('',#18527,0.249999570396437);
#581=CYLINDRICAL_SURFACE('',#18528,0.250000000000004);
#582=CYLINDRICAL_SURFACE('',#18554,17.5);
#583=CYLINDRICAL_SURFACE('',#18557,19.5);
#584=CYLINDRICAL_SURFACE('',#18559,31.5);
#585=CYLINDRICAL_SURFACE('',#18565,4.);
#586=CYLINDRICAL_SURFACE('',#18568,4.);
#587=CYLINDRICAL_SURFACE('',#18571,4.);
#588=CYLINDRICAL_SURFACE('',#18574,4.);
#589=CYLINDRICAL_SURFACE('',#18577,4.);
#590=CYLINDRICAL_SURFACE('',#18580,4.);
#591=CYLINDRICAL_SURFACE('',#18644,0.800000000000002);
#592=CYLINDRICAL_SURFACE('',#18646,0.800000000000002);
#593=CYLINDRICAL_SURFACE('',#18648,0.799999999999995);
#594=CYLINDRICAL_SURFACE('',#18651,0.799999999999995);
#595=CYLINDRICAL_SURFACE('',#18661,1.6);
#596=CYLINDRICAL_SURFACE('',#18663,1.15469920262284);
#597=CYLINDRICAL_SURFACE('',#18666,1.6);
#598=CYLINDRICAL_SURFACE('',#18668,1.6);
#599=CYLINDRICAL_SURFACE('',#18670,1.6);
#600=CYLINDRICAL_SURFACE('',#18672,1.33321558059984);
#601=CYLINDRICAL_SURFACE('',#18675,1.32106757713908);
#602=CYLINDRICAL_SURFACE('',#18678,2.1);
#603=CYLINDRICAL_SURFACE('',#18680,1.6);
#604=CYLINDRICAL_SURFACE('',#18682,1.6);
#605=CYLINDRICAL_SURFACE('',#18684,1.6);
#606=CYLINDRICAL_SURFACE('',#18686,1.6);
#607=CYLINDRICAL_SURFACE('',#18688,1.6);
#608=CYLINDRICAL_SURFACE('',#18690,1.6);
#609=CYLINDRICAL_SURFACE('',#18692,1.6);
#610=CYLINDRICAL_SURFACE('',#18694,1.6);
#611=CYLINDRICAL_SURFACE('',#18700,7.25609345692882);
#612=CYLINDRICAL_SURFACE('',#18705,8.3116573007006);
#613=CYLINDRICAL_SURFACE('',#18709,7.62932104676364);
#614=CYLINDRICAL_SURFACE('',#18727,0.233315989528693);
#615=CYLINDRICAL_SURFACE('',#18730,41.9475849136215);
#616=CYLINDRICAL_SURFACE('',#18743,2.);
#617=CYLINDRICAL_SURFACE('',#18746,2.);
#618=CYLINDRICAL_SURFACE('',#18758,0.399999999999998);
#619=CYLINDRICAL_SURFACE('',#18761,0.399999999999998);
#620=CYLINDRICAL_SURFACE('',#18764,0.399999999999998);
#621=CYLINDRICAL_SURFACE('',#18767,0.399999999999998);
#622=CYLINDRICAL_SURFACE('',#18788,1.60000000000001);
#623=CYLINDRICAL_SURFACE('',#18790,1.60000000000001);
#624=CYLINDRICAL_SURFACE('',#18791,1.60000000000001);
#625=CYLINDRICAL_SURFACE('',#18792,1.60000000000001);
#626=CYLINDRICAL_SURFACE('',#18793,1.60000000000001);
#627=CYLINDRICAL_SURFACE('',#18794,1.60000000000001);
#628=CYLINDRICAL_SURFACE('',#18795,1.60000000000001);
#629=CYLINDRICAL_SURFACE('',#18796,1.60000000000001);
#630=CYLINDRICAL_SURFACE('',#18797,1.60000000000001);
#631=CYLINDRICAL_SURFACE('',#18798,1.60000000000001);
#632=CYLINDRICAL_SURFACE('',#18799,1.60000000000001);
#633=CYLINDRICAL_SURFACE('',#18800,1.60000000000001);
#634=CYLINDRICAL_SURFACE('',#18801,1.60000000000001);
#635=CYLINDRICAL_SURFACE('',#18802,1.60000000000001);
#636=CYLINDRICAL_SURFACE('',#18803,1.60000000000001);
#637=CYLINDRICAL_SURFACE('',#18804,1.60000000000001);
#638=CYLINDRICAL_SURFACE('',#18805,1.60000000000001);
#639=CYLINDRICAL_SURFACE('',#18806,1.60000000000001);
#640=CYLINDRICAL_SURFACE('',#18807,1.60000000000001);
#641=CYLINDRICAL_SURFACE('',#18809,1.59999999999791);
#642=CYLINDRICAL_SURFACE('',#18812,1.22111388749974);
#643=CYLINDRICAL_SURFACE('',#18813,1.22111388749974);
#644=CYLINDRICAL_SURFACE('',#18814,1.22111388749974);
#645=CYLINDRICAL_SURFACE('',#18815,1.22111388749974);
#646=CYLINDRICAL_SURFACE('',#18816,1.22111388749974);
#647=CYLINDRICAL_SURFACE('',#18817,1.22111388749974);
#648=CYLINDRICAL_SURFACE('',#18818,1.22111388749974);
#649=CYLINDRICAL_SURFACE('',#18819,1.22111388749974);
#650=CYLINDRICAL_SURFACE('',#18820,1.22111388749974);
#651=CYLINDRICAL_SURFACE('',#18821,1.22111388749974);
#652=CYLINDRICAL_SURFACE('',#18822,1.22111388749974);
#653=CYLINDRICAL_SURFACE('',#18823,1.22111388749974);
#654=CYLINDRICAL_SURFACE('',#18824,1.22111388749974);
#655=CYLINDRICAL_SURFACE('',#18825,1.22111388749974);
#656=CYLINDRICAL_SURFACE('',#18826,1.22111388749974);
#657=CYLINDRICAL_SURFACE('',#18827,1.22111388749974);
#658=CYLINDRICAL_SURFACE('',#18828,1.22111388749974);
#659=CYLINDRICAL_SURFACE('',#18829,1.22111388749974);
#660=CYLINDRICAL_SURFACE('',#18830,1.22111388749974);
#661=CYLINDRICAL_SURFACE('',#18831,1.22111388749974);
#662=CYLINDRICAL_SURFACE('',#18832,8.49999999999999);
#663=CYLINDRICAL_SURFACE('',#18834,8.49999999999999);
#664=CYLINDRICAL_SURFACE('',#18835,8.49999999999999);
#665=CYLINDRICAL_SURFACE('',#18836,7.68810118749996);
#666=CYLINDRICAL_SURFACE('',#18837,7.68810118749996);
#667=CYLINDRICAL_SURFACE('',#18838,7.68810118749996);
#668=CYLINDRICAL_SURFACE('',#18839,7.68810118749996);
#669=CYLINDRICAL_SURFACE('',#18840,7.68810118749996);
#670=CYLINDRICAL_SURFACE('',#18841,7.68810118749996);
#671=CYLINDRICAL_SURFACE('',#18842,7.68810118749996);
#672=CYLINDRICAL_SURFACE('',#18843,7.68810118749996);
#673=CYLINDRICAL_SURFACE('',#18844,8.1);
#674=CYLINDRICAL_SURFACE('',#18846,8.1);
#675=CYLINDRICAL_SURFACE('',#18847,8.1);
#676=CYLINDRICAL_SURFACE('',#18848,8.1);
#677=CYLINDRICAL_SURFACE('',#18849,8.1);
#678=CYLINDRICAL_SURFACE('',#18871,14.);
#679=CYLINDRICAL_SURFACE('',#18876,12.);
#680=CYLINDRICAL_SURFACE('',#18882,8.1);
#681=CYLINDRICAL_SURFACE('',#18892,14.);
#682=CYLINDRICAL_SURFACE('',#18894,14.);
#683=CYLINDRICAL_SURFACE('',#18896,14.);
#684=CYLINDRICAL_SURFACE('',#18904,6.00000000000001);
#685=CYLINDRICAL_SURFACE('',#18907,8.49999999999999);
#686=CYLINDRICAL_SURFACE('',#18909,7.68810118749996);
#687=CYLINDRICAL_SURFACE('',#18918,4.75);
#688=CYLINDRICAL_SURFACE('',#18921,7.00000000000001);
#689=CYLINDRICAL_SURFACE('',#18927,10.);
#690=CYLINDRICAL_SURFACE('',#18948,1.2500000000005);
#691=CYLINDRICAL_SURFACE('',#18951,1.25000000000059);
#692=CYLINDRICAL_SURFACE('',#18955,1.25000000000024);
#693=CYLINDRICAL_SURFACE('',#18959,1.24999999999999);
#694=CYLINDRICAL_SURFACE('',#18963,6.00000000000001);
#695=CYLINDRICAL_SURFACE('',#19057,8.49999999999999);
#696=CYLINDRICAL_SURFACE('',#19062,3.99999999999999);
#697=CYLINDRICAL_SURFACE('',#19065,1.22111388749974);
#698=CYLINDRICAL_SURFACE('',#19068,1.59999999999791);
#699=CYLINDRICAL_SURFACE('',#19070,1.59999999999791);
#700=CYLINDRICAL_SURFACE('',#19081,3.99999999999999);
#701=CYLINDRICAL_SURFACE('',#19084,1.60000000000001);
#702=CYLINDRICAL_SURFACE('',#19086,1.4);
#703=CYLINDRICAL_SURFACE('',#19092,1.4);
#704=CYLINDRICAL_SURFACE('',#19121,1.6);
#705=CYLINDRICAL_SURFACE('',#19123,1.6);
#706=CYLINDRICAL_SURFACE('',#19138,2.);
#707=CYLINDRICAL_SURFACE('',#19139,2.);
#708=CYLINDRICAL_SURFACE('',#19147,1.6);
#709=CYLINDRICAL_SURFACE('',#19149,1.6);
#710=CYLINDRICAL_SURFACE('',#19175,4.);
#711=CYLINDRICAL_SURFACE('',#19176,1.6);
#712=CYLINDRICAL_SURFACE('',#19178,1.6);
#713=CYLINDRICAL_SURFACE('',#19179,1.6);
#714=CYLINDRICAL_SURFACE('',#19180,1.6);
#715=CYLINDRICAL_SURFACE('',#19181,1.6);
#716=CYLINDRICAL_SURFACE('',#19182,1.6);
#717=CYLINDRICAL_SURFACE('',#19183,1.6);
#718=CYLINDRICAL_SURFACE('',#19184,1.6);
#719=CYLINDRICAL_SURFACE('',#19185,1.6);
#720=CYLINDRICAL_SURFACE('',#19186,1.6);
#721=CYLINDRICAL_SURFACE('',#19187,1.6);
#722=CYLINDRICAL_SURFACE('',#19188,1.6);
#723=CYLINDRICAL_SURFACE('',#19189,1.6);
#724=CYLINDRICAL_SURFACE('',#19190,1.6);
#725=CYLINDRICAL_SURFACE('',#19192,1.22111388750008);
#726=CYLINDRICAL_SURFACE('',#19193,1.22111388750008);
#727=CYLINDRICAL_SURFACE('',#19194,1.22111388750008);
#728=CYLINDRICAL_SURFACE('',#19195,1.22111388750008);
#729=CYLINDRICAL_SURFACE('',#19196,1.22111388750008);
#730=CYLINDRICAL_SURFACE('',#19197,1.22111388750008);
#731=CYLINDRICAL_SURFACE('',#19198,1.22111388750008);
#732=CYLINDRICAL_SURFACE('',#19199,1.22111388750008);
#733=CYLINDRICAL_SURFACE('',#19200,1.22111388750008);
#734=CYLINDRICAL_SURFACE('',#19201,1.22111388750008);
#735=CYLINDRICAL_SURFACE('',#19202,1.22111388750008);
#736=CYLINDRICAL_SURFACE('',#19203,1.22111388750008);
#737=CYLINDRICAL_SURFACE('',#19204,1.22111388750008);
#738=CYLINDRICAL_SURFACE('',#19205,1.22111388750008);
#739=CYLINDRICAL_SURFACE('',#19206,1.60000000000001);
#740=CYLINDRICAL_SURFACE('',#19209,1.49172584788676);
#741=CYLINDRICAL_SURFACE('',#19212,1.04190416256385);
#742=CYLINDRICAL_SURFACE('',#19235,3.25);
#743=CYLINDRICAL_SURFACE('',#19236,12.);
#744=CYLINDRICAL_SURFACE('',#19242,1.59999999999981);
#745=CYLINDRICAL_SURFACE('',#19245,1.22111388750008);
#746=CYLINDRICAL_SURFACE('',#19248,1.59999999999981);
#747=CYLINDRICAL_SURFACE('',#19258,1.6);
#748=CYLINDRICAL_SURFACE('',#19268,5.);
#749=CYLINDRICAL_SURFACE('',#19269,7.);
#750=CYLINDRICAL_SURFACE('',#19271,4.22087352428905);
#751=CYLINDRICAL_SURFACE('',#19274,1.6);
#752=CYLINDRICAL_SURFACE('',#19279,4.5);
#753=CYLINDRICAL_SURFACE('',#19294,5.14310210370206);
#754=CYLINDRICAL_SURFACE('',#19317,0.699999999999999);
#755=CYLINDRICAL_SURFACE('',#19318,0.699999999999999);
#756=CYLINDRICAL_SURFACE('',#19319,0.7);
#757=CYLINDRICAL_SURFACE('',#19320,0.7);
#758=CYLINDRICAL_SURFACE('',#19325,0.599999999999998);
#759=CYLINDRICAL_SURFACE('',#19326,0.599999999999998);
#760=CYLINDRICAL_SURFACE('',#19327,0.599999999999998);
#761=CYLINDRICAL_SURFACE('',#19328,0.599999999999998);
#762=CYLINDRICAL_SURFACE('',#19338,0.499999999999999);
#763=CYLINDRICAL_SURFACE('',#19341,0.500000000000004);
#764=CYLINDRICAL_SURFACE('',#19343,0.500000000000005);
#765=CYLINDRICAL_SURFACE('',#19345,0.500000000000005);
#766=CYLINDRICAL_SURFACE('',#19347,0.500000000000004);
#767=CYLINDRICAL_SURFACE('',#19349,0.499999999999999);
#768=CYLINDRICAL_SURFACE('',#19350,4.);
#769=CYLINDRICAL_SURFACE('',#19353,1.6);
#770=CYLINDRICAL_SURFACE('',#19356,4.50000000000007);
#771=CYLINDRICAL_SURFACE('',#19397,4.11168229960152);
#772=CYLINDRICAL_SURFACE('',#19406,1.49172584788676);
#773=CYLINDRICAL_SURFACE('',#19410,4.6918515041613);
#774=CYLINDRICAL_SURFACE('',#19417,0.338583852498097);
#775=CYLINDRICAL_SURFACE('',#19423,2.81299719163292);
#776=FACE_BOUND('',#2459,.T.);
#777=FACE_BOUND('',#2460,.T.);
#778=FACE_BOUND('',#2461,.T.);
#779=FACE_BOUND('',#2462,.T.);
#780=FACE_BOUND('',#2463,.T.);
#781=FACE_BOUND('',#2464,.T.);
#782=FACE_BOUND('',#2465,.T.);
#783=FACE_BOUND('',#2466,.T.);
#784=FACE_BOUND('',#2467,.T.);
#785=FACE_BOUND('',#2468,.T.);
#786=FACE_BOUND('',#2469,.T.);
#787=FACE_BOUND('',#2470,.T.);
#788=FACE_BOUND('',#2471,.T.);
#789=FACE_BOUND('',#2472,.T.);
#790=FACE_BOUND('',#2473,.T.);
#791=FACE_BOUND('',#2474,.T.);
#792=FACE_BOUND('',#2475,.T.);
#793=FACE_BOUND('',#2476,.T.);
#794=FACE_BOUND('',#2477,.T.);
#795=FACE_BOUND('',#2478,.T.);
#796=FACE_BOUND('',#2479,.T.);
#797=FACE_BOUND('',#2480,.T.);
#798=FACE_BOUND('',#2481,.T.);
#799=FACE_BOUND('',#2482,.T.);
#800=FACE_BOUND('',#2483,.T.);
#801=FACE_BOUND('',#2484,.T.);
#802=FACE_BOUND('',#2485,.T.);
#803=FACE_BOUND('',#2486,.T.);
#804=FACE_BOUND('',#2487,.T.);
#805=FACE_BOUND('',#2488,.T.);
#806=FACE_BOUND('',#2489,.T.);
#807=FACE_BOUND('',#2490,.T.);
#808=FACE_BOUND('',#2491,.T.);
#809=FACE_BOUND('',#2492,.T.);
#810=FACE_BOUND('',#2493,.T.);
#811=FACE_BOUND('',#2494,.T.);
#812=FACE_BOUND('',#2495,.T.);
#813=FACE_BOUND('',#2496,.T.);
#814=FACE_BOUND('',#2497,.T.);
#815=FACE_BOUND('',#2498,.T.);
#816=FACE_BOUND('',#2499,.T.);
#817=FACE_BOUND('',#2500,.T.);
#818=FACE_BOUND('',#2501,.T.);
#819=FACE_BOUND('',#2502,.T.);
#820=FACE_BOUND('',#2503,.T.);
#821=FACE_BOUND('',#2504,.T.);
#822=FACE_BOUND('',#2505,.T.);
#823=FACE_BOUND('',#2506,.T.);
#824=FACE_BOUND('',#2507,.T.);
#825=FACE_BOUND('',#2508,.T.);
#826=FACE_BOUND('',#2509,.T.);
#827=FACE_BOUND('',#2510,.T.);
#828=FACE_BOUND('',#2512,.T.);
#829=FACE_BOUND('',#2513,.T.);
#830=FACE_BOUND('',#2514,.T.);
#831=FACE_BOUND('',#2515,.T.);
#832=FACE_BOUND('',#2516,.T.);
#833=FACE_BOUND('',#2517,.T.);
#834=FACE_BOUND('',#2518,.T.);
#835=FACE_BOUND('',#2519,.T.);
#836=FACE_BOUND('',#2520,.T.);
#837=FACE_BOUND('',#2521,.T.);
#838=FACE_BOUND('',#2522,.T.);
#839=FACE_BOUND('',#2523,.T.);
#840=FACE_BOUND('',#2524,.T.);
#841=FACE_BOUND('',#2525,.T.);
#842=FACE_BOUND('',#2526,.T.);
#843=FACE_BOUND('',#2527,.T.);
#844=FACE_BOUND('',#2528,.T.);
#845=FACE_BOUND('',#2529,.T.);
#846=FACE_BOUND('',#2530,.T.);
#847=FACE_BOUND('',#2531,.T.);
#848=FACE_BOUND('',#2532,.T.);
#849=FACE_BOUND('',#2533,.T.);
#850=FACE_BOUND('',#2534,.T.);
#851=FACE_BOUND('',#2535,.T.);
#852=FACE_BOUND('',#2536,.T.);
#853=FACE_BOUND('',#2537,.T.);
#854=FACE_BOUND('',#2538,.T.);
#855=FACE_BOUND('',#2539,.T.);
#856=FACE_BOUND('',#2540,.T.);
#857=FACE_BOUND('',#2541,.T.);
#858=FACE_BOUND('',#2542,.T.);
#859=FACE_BOUND('',#2543,.T.);
#860=FACE_BOUND('',#2544,.T.);
#861=FACE_BOUND('',#2545,.T.);
#862=FACE_BOUND('',#2546,.T.);
#863=FACE_BOUND('',#2547,.T.);
#864=FACE_BOUND('',#2548,.T.);
#865=FACE_BOUND('',#2549,.T.);
#866=FACE_BOUND('',#2550,.T.);
#867=FACE_BOUND('',#2551,.T.);
#868=FACE_BOUND('',#2552,.T.);
#869=FACE_BOUND('',#2553,.T.);
#870=FACE_BOUND('',#2554,.T.);
#871=FACE_BOUND('',#2555,.T.);
#872=FACE_BOUND('',#2556,.T.);
#873=FACE_BOUND('',#2557,.T.);
#874=FACE_BOUND('',#2558,.T.);
#875=FACE_BOUND('',#2559,.T.);
#876=FACE_BOUND('',#2560,.T.);
#877=FACE_BOUND('',#2561,.T.);
#878=FACE_BOUND('',#2562,.T.);
#879=FACE_BOUND('',#2563,.T.);
#880=FACE_BOUND('',#2725,.T.);
#881=FACE_BOUND('',#2780,.T.);
#882=FACE_BOUND('',#2781,.T.);
#883=FACE_BOUND('',#2788,.T.);
#884=FACE_BOUND('',#2789,.T.);
#885=FACE_BOUND('',#2822,.T.);
#886=FACE_BOUND('',#2825,.T.);
#887=FACE_BOUND('',#2828,.T.);
#888=FACE_BOUND('',#2832,.T.);
#889=FACE_BOUND('',#2913,.T.);
#890=FACE_BOUND('',#2920,.T.);
#891=FACE_BOUND('',#2999,.T.);
#892=FACE_BOUND('',#3000,.T.);
#893=FACE_BOUND('',#3001,.T.);
#894=FACE_BOUND('',#3002,.T.);
#895=FACE_BOUND('',#3003,.T.);
#896=FACE_BOUND('',#3004,.T.);
#897=FACE_BOUND('',#3005,.T.);
#898=FACE_BOUND('',#3006,.T.);
#899=FACE_BOUND('',#3007,.T.);
#900=FACE_BOUND('',#3008,.T.);
#901=FACE_BOUND('',#3009,.T.);
#902=FACE_BOUND('',#3010,.T.);
#903=FACE_BOUND('',#3011,.T.);
#904=FACE_BOUND('',#3012,.T.);
#905=FACE_BOUND('',#3013,.T.);
#906=FACE_BOUND('',#3014,.T.);
#907=FACE_BOUND('',#3015,.T.);
#908=FACE_BOUND('',#3017,.T.);
#909=FACE_BOUND('',#3018,.T.);
#910=FACE_BOUND('',#3019,.T.);
#911=FACE_BOUND('',#3020,.T.);
#912=FACE_BOUND('',#3021,.T.);
#913=FACE_BOUND('',#3022,.T.);
#914=FACE_BOUND('',#3023,.T.);
#915=FACE_BOUND('',#3024,.T.);
#916=FACE_BOUND('',#3025,.T.);
#917=FACE_BOUND('',#3026,.T.);
#918=FACE_BOUND('',#3027,.T.);
#919=FACE_BOUND('',#3028,.T.);
#920=FACE_BOUND('',#3029,.T.);
#921=FACE_BOUND('',#3030,.T.);
#922=FACE_BOUND('',#3031,.T.);
#923=FACE_BOUND('',#3032,.T.);
#924=FACE_BOUND('',#3033,.T.);
#925=FACE_BOUND('',#3049,.T.);
#926=FACE_BOUND('',#3050,.T.);
#927=FACE_BOUND('',#3154,.T.);
#928=FACE_BOUND('',#3168,.T.);
#929=FACE_BOUND('',#3178,.T.);
#930=FACE_BOUND('',#3180,.T.);
#931=FACE_BOUND('',#3183,.T.);
#932=FACE_BOUND('',#3284,.T.);
#933=FACE_BOUND('',#3285,.T.);
#934=FACE_BOUND('',#3286,.T.);
#935=FACE_BOUND('',#3287,.T.);
#936=FACE_BOUND('',#3288,.T.);
#937=FACE_BOUND('',#3290,.T.);
#938=FACE_BOUND('',#3293,.T.);
#939=FACE_BOUND('',#3295,.T.);
#940=FACE_BOUND('',#3310,.T.);
#941=FACE_BOUND('',#3312,.T.);
#942=FACE_BOUND('',#3354,.T.);
#943=FACE_BOUND('',#3355,.T.);
#944=FACE_BOUND('',#3358,.T.);
#945=FACE_BOUND('',#3359,.T.);
#946=FACE_BOUND('',#3361,.T.);
#947=FACE_BOUND('',#3362,.T.);
#948=FACE_BOUND('',#3367,.T.);
#949=FACE_BOUND('',#3371,.T.);
#950=FACE_BOUND('',#3373,.T.);
#951=FACE_BOUND('',#3381,.T.);
#952=FACE_BOUND('',#3382,.T.);
#953=FACE_BOUND('',#3387,.T.);
#954=FACE_BOUND('',#3396,.T.);
#955=FACE_BOUND('',#3397,.T.);
#956=FACE_BOUND('',#3399,.T.);
#957=FACE_BOUND('',#3440,.T.);
#958=FACE_BOUND('',#3442,.T.);
#959=FACE_BOUND('',#3444,.T.);
#960=FACE_BOUND('',#3456,.T.);
#961=FACE_BOUND('',#3466,.T.);
#962=FACE_BOUND('',#3467,.T.);
#963=FACE_BOUND('',#3470,.T.);
#964=FACE_BOUND('',#3471,.T.);
#965=FACE_BOUND('',#3488,.T.);
#966=FACE_BOUND('',#3497,.T.);
#967=FACE_BOUND('',#3503,.T.);
#968=FACE_BOUND('',#3520,.T.);
#969=FACE_BOUND('',#3566,.T.);
#970=FACE_BOUND('',#3568,.T.);
#971=FACE_BOUND('',#3583,.T.);
#972=FACE_BOUND('',#3585,.T.);
#973=CIRCLE('',#17918,0.750000000000001);
#974=CIRCLE('',#17919,0.750000000000001);
#975=CIRCLE('',#17920,0.750000000000001);
#976=CIRCLE('',#17921,0.75);
#977=CIRCLE('',#17922,0.75);
#978=CIRCLE('',#17923,0.75);
#979=CIRCLE('',#17924,0.75);
#980=CIRCLE('',#17925,0.750000000000001);
#981=CIRCLE('',#17926,0.750000000000001);
#982=CIRCLE('',#17927,0.750000000000001);
#983=CIRCLE('',#17928,0.750000000000001);
#984=CIRCLE('',#17929,0.750000000000001);
#985=CIRCLE('',#17930,0.750000000000001);
#986=CIRCLE('',#17931,0.750000000000001);
#987=CIRCLE('',#17932,0.750000000000001);
#988=CIRCLE('',#17933,0.750000000000001);
#989=CIRCLE('',#17934,0.750000000000001);
#990=CIRCLE('',#17935,0.750000000000001);
#991=CIRCLE('',#17936,0.750000000000001);
#992=CIRCLE('',#17937,0.750000000000001);
#993=CIRCLE('',#17938,0.750000000000001);
#994=CIRCLE('',#17939,0.750000000000001);
#995=CIRCLE('',#17940,0.750000000000001);
#996=CIRCLE('',#17941,0.750000000000001);
#997=CIRCLE('',#17942,0.750000000000001);
#998=CIRCLE('',#17943,0.750000000000001);
#999=CIRCLE('',#17945,0.750000000000001);
#1000=CIRCLE('',#17946,0.750000000000001);
#1001=CIRCLE('',#17947,0.750000000000001);
#1002=CIRCLE('',#17948,0.750000000000001);
#1003=CIRCLE('',#17949,0.750000000000001);
#1004=CIRCLE('',#17950,0.750000000000001);
#1005=CIRCLE('',#17951,0.750000000000001);
#1006=CIRCLE('',#17952,0.750000000000001);
#1007=CIRCLE('',#17953,0.750000000000001);
#1008=CIRCLE('',#17954,0.750000000000001);
#1009=CIRCLE('',#17955,0.750000000000001);
#1010=CIRCLE('',#17956,0.750000000000001);
#1011=CIRCLE('',#17957,0.750000000000001);
#1012=CIRCLE('',#17958,0.750000000000001);
#1013=CIRCLE('',#17959,0.750000000000001);
#1014=CIRCLE('',#17960,0.750000000000001);
#1015=CIRCLE('',#17961,0.750000000000001);
#1016=CIRCLE('',#17962,0.750000000000001);
#1017=CIRCLE('',#17963,0.750000000000001);
#1018=CIRCLE('',#17964,0.75);
#1019=CIRCLE('',#17965,0.75);
#1020=CIRCLE('',#17966,0.75);
#1021=CIRCLE('',#17967,0.75);
#1022=CIRCLE('',#17968,0.750000000000001);
#1023=CIRCLE('',#17969,0.750000000000001);
#1024=CIRCLE('',#17970,0.750000000000001);
#1025=CIRCLE('',#18127,0.5);
#1026=CIRCLE('',#18128,1.);
#1027=CIRCLE('',#18129,0.5);
#1028=CIRCLE('',#18130,0.5);
#1029=CIRCLE('',#18132,0.5);
#1030=CIRCLE('',#18133,0.5);
#1031=CIRCLE('',#18135,0.5);
#1032=CIRCLE('',#18137,0.5);
#1033=CIRCLE('',#18139,0.5);
#1034=CIRCLE('',#18141,0.5);
#1035=CIRCLE('',#18142,0.5);
#1036=CIRCLE('',#18143,0.5);
#1037=CIRCLE('',#18144,0.5);
#1038=CIRCLE('',#18145,0.5);
#1039=CIRCLE('',#18146,1.);
#1040=CIRCLE('',#18148,0.5);
#1041=CIRCLE('',#18150,0.5);
#1042=CIRCLE('',#18155,0.5);
#1043=CIRCLE('',#18158,0.5);
#1044=CIRCLE('',#18159,0.5);
#1045=CIRCLE('',#18161,0.5);
#1046=CIRCLE('',#18162,0.5);
#1047=CIRCLE('',#18168,0.5);
#1048=CIRCLE('',#18169,0.5);
#1049=CIRCLE('',#18171,0.5);
#1050=CIRCLE('',#18172,0.5);
#1051=CIRCLE('',#18174,0.5);
#1052=CIRCLE('',#18175,0.5);
#1053=CIRCLE('',#18177,0.5);
#1054=CIRCLE('',#18178,0.5);
#1055=CIRCLE('',#18198,0.5);
#1056=CIRCLE('',#18199,0.5);
#1057=CIRCLE('',#18201,0.5);
#1058=CIRCLE('',#18202,0.5);
#1059=CIRCLE('',#18204,0.5);
#1060=CIRCLE('',#18205,0.5);
#1061=CIRCLE('',#18207,0.5);
#1062=CIRCLE('',#18208,0.5);
#1063=CIRCLE('',#18219,1.76114216495771);
#1064=CIRCLE('',#18220,2.15235845279182);
#1065=CIRCLE('',#18222,2.15235845279183);
#1066=CIRCLE('',#18223,1.76114216495771);
#1067=CIRCLE('',#18226,1.76114216495771);
#1068=CIRCLE('',#18227,2.15235845279182);
#1069=CIRCLE('',#18229,1.76114216495771);
#1070=CIRCLE('',#18230,2.15235845279182);
#1071=CIRCLE('',#18232,1.6);
#1072=CIRCLE('',#18233,1.6);
#1073=CIRCLE('',#18236,1.6);
#1074=CIRCLE('',#18237,1.6);
#1075=CIRCLE('',#18240,1.6);
#1076=CIRCLE('',#18241,1.6);
#1077=CIRCLE('',#18244,1.6);
#1078=CIRCLE('',#18245,1.6);
#1079=CIRCLE('',#18248,1.76114216495771);
#1080=CIRCLE('',#18251,2.15235845279182);
#1081=CIRCLE('',#18254,2.15235845279182);
#1082=CIRCLE('',#18263,1.76114216495771);
#1083=CIRCLE('',#18272,0.250000000000003);
#1084=CIRCLE('',#18273,0.249999999999998);
#1085=CIRCLE('',#18274,0.250000000000004);
#1086=CIRCLE('',#18276,0.249999999999996);
#1087=CIRCLE('',#18277,0.25);
#1088=CIRCLE('',#18278,0.249999999999993);
#1089=CIRCLE('',#18280,0.249999999999998);
#1090=CIRCLE('',#18281,0.250000000000003);
#1091=CIRCLE('',#18282,0.250000000000001);
#1092=CIRCLE('',#18284,0.249999999999998);
#1093=CIRCLE('',#18285,0.249999999999997);
#1094=CIRCLE('',#18286,0.249999999999998);
#1095=CIRCLE('',#18288,0.250000000000002);
#1096=CIRCLE('',#18289,0.250000000000006);
#1097=CIRCLE('',#18290,0.25);
#1098=CIRCLE('',#18292,0.249999999999995);
#1099=CIRCLE('',#18293,0.249999999999998);
#1100=CIRCLE('',#18294,0.249999999999998);
#1101=CIRCLE('',#18296,0.250000000000003);
#1102=CIRCLE('',#18297,0.249999999999997);
#1103=CIRCLE('',#18298,0.250000000000005);
#1104=CIRCLE('',#18300,0.250000000000004);
#1105=CIRCLE('',#18301,0.25);
#1106=CIRCLE('',#18302,0.249999999999998);
#1107=CIRCLE('',#18304,0.249999999999998);
#1108=CIRCLE('',#18305,0.250000000000003);
#1109=CIRCLE('',#18306,0.250000000000007);
#1110=CIRCLE('',#18308,0.250000000000005);
#1111=CIRCLE('',#18309,0.250000000000003);
#1112=CIRCLE('',#18310,0.249999999999998);
#1113=CIRCLE('',#18312,15.8);
#1114=CIRCLE('',#18313,0.3);
#1115=CIRCLE('',#18314,15.5);
#1116=CIRCLE('',#18316,31.5);
#1117=CIRCLE('',#18317,31.5);
#1118=CIRCLE('',#18318,0.3);
#1119=CIRCLE('',#18319,31.2047362517505);
#1120=CIRCLE('',#18321,12.5);
#1121=CIRCLE('',#18322,0.3);
#1122=CIRCLE('',#18323,12.7952637482494);
#1123=CIRCLE('',#18324,12.7952637482494);
#1124=CIRCLE('',#18326,10.5);
#1125=CIRCLE('',#18327,0.3);
#1126=CIRCLE('',#18328,10.2);
#1127=CIRCLE('',#18330,10.5);
#1128=CIRCLE('',#18331,0.3);
#1129=CIRCLE('',#18332,10.2);
#1130=CIRCLE('',#18333,10.2);
#1131=CIRCLE('',#18335,31.5);
#1132=CIRCLE('',#18336,0.3);
#1133=CIRCLE('',#18337,31.2);
#1134=CIRCLE('',#18339,18.2);
#1135=CIRCLE('',#18340,0.3);
#1136=CIRCLE('',#18341,17.9);
#1137=CIRCLE('',#18343,17.5127413251518);
#1138=CIRCLE('',#18344,0.3);
#1139=CIRCLE('',#18345,17.2130371832119);
#1140=CIRCLE('',#18347,16.1);
#1141=CIRCLE('',#18348,0.3);
#1142=CIRCLE('',#18349,15.8);
#1143=CIRCLE('',#18352,17.9);
#1144=CIRCLE('',#18353,17.9);
#1145=CIRCLE('',#18354,17.9);
#1146=CIRCLE('',#18355,17.9);
#1147=CIRCLE('',#18356,17.9);
#1148=CIRCLE('',#18357,17.9);
#1149=CIRCLE('',#18358,17.9);
#1150=CIRCLE('',#18359,17.9);
#1151=CIRCLE('',#18360,17.9);
#1152=CIRCLE('',#18361,17.9);
#1153=CIRCLE('',#18362,17.9);
#1154=CIRCLE('',#18364,17.6796049747715);
#1155=CIRCLE('',#18365,17.6796049747715);
#1156=CIRCLE('',#18366,17.6796049747715);
#1157=CIRCLE('',#18367,17.6796049747715);
#1158=CIRCLE('',#18368,17.6796049747715);
#1159=CIRCLE('',#18369,17.6796049747715);
#1160=CIRCLE('',#18370,17.6796049747715);
#1161=CIRCLE('',#18376,12.5);
#1162=CIRCLE('',#18381,31.5);
#1163=CIRCLE('',#18382,31.5);
#1164=CIRCLE('',#18383,0.25);
#1165=CIRCLE('',#18384,31.25);
#1166=CIRCLE('',#18386,19.75);
#1167=CIRCLE('',#18387,0.25);
#1168=CIRCLE('',#18388,19.5);
#1169=CIRCLE('',#18390,17.5);
#1170=CIRCLE('',#18391,17.5);
#1171=CIRCLE('',#18392,0.25);
#1172=CIRCLE('',#18393,17.5001812086856);
#1173=CIRCLE('',#18395,0.250000000000003);
#1174=CIRCLE('',#18397,0.250000000000004);
#1175=CIRCLE('',#18398,0.249999999999994);
#1176=CIRCLE('',#18400,18.1406575306034);
#1177=CIRCLE('',#18401,0.250000000000002);
#1178=CIRCLE('',#18404,0.249999999999998);
#1179=CIRCLE('',#18406,19.25);
#1180=CIRCLE('',#18407,19.5);
#1181=CIRCLE('',#18409,0.250000000000001);
#1182=CIRCLE('',#18410,0.250000000000003);
#1183=CIRCLE('',#18412,17.759705149651);
#1184=CIRCLE('',#18413,17.5098863583366);
#1185=CIRCLE('',#18415,19.5);
#1186=CIRCLE('',#18416,19.25);
#1187=CIRCLE('',#18421,0.249999999999998);
#1188=CIRCLE('',#18422,0.249999999999998);
#1189=CIRCLE('',#18424,0.249999999999998);
#1190=CIRCLE('',#18426,17.5098863583366);
#1191=CIRCLE('',#18427,17.759705149651);
#1192=CIRCLE('',#18429,0.249999999999995);
#1193=CIRCLE('',#18430,0.250000000000003);
#1194=CIRCLE('',#18432,19.25);
#1195=CIRCLE('',#18433,19.5);
#1196=CIRCLE('',#18436,0.249999999999993);
#1197=CIRCLE('',#18437,18.1406575306034);
#1198=CIRCLE('',#18440,19.5);
#1199=CIRCLE('',#18441,19.25);
#1200=CIRCLE('',#18443,0.249999999999998);
#1201=CIRCLE('',#18444,0.249999999999998);
#1202=CIRCLE('',#18446,0.249999999999999);
#1203=CIRCLE('',#18447,0.25);
#1204=CIRCLE('',#18449,0.250000000000003);
#1205=CIRCLE('',#18450,0.250000000000005);
#1206=CIRCLE('',#18453,18.1406575306034);
#1207=CIRCLE('',#18457,0.249999999999998);
#1208=CIRCLE('',#18459,0.250000000000002);
#1209=CIRCLE('',#18460,19.25);
#1210=CIRCLE('',#18461,19.5);
#1211=CIRCLE('',#18463,17.759705149651);
#1212=CIRCLE('',#18464,17.5098863583366);
#1213=CIRCLE('',#18466,19.5);
#1214=CIRCLE('',#18467,19.25);
#1215=CIRCLE('',#18469,0.249999999999996);
#1216=CIRCLE('',#18470,0.250000000000006);
#1217=CIRCLE('',#18474,0.249999999999999);
#1218=CIRCLE('',#18476,0.249999999999998);
#1219=CIRCLE('',#18478,0.249999999999996);
#1220=CIRCLE('',#18480,17.5098863583366);
#1221=CIRCLE('',#18481,17.759705149651);
#1222=CIRCLE('',#18483,0.249999999999997);
#1223=CIRCLE('',#18484,0.249999999999998);
#1224=CIRCLE('',#18486,19.25);
#1225=CIRCLE('',#18487,19.5);
#1226=CIRCLE('',#18489,0.250000000000002);
#1227=CIRCLE('',#18491,18.1406575306034);
#1228=CIRCLE('',#18494,0.250000000000001);
#1229=CIRCLE('',#18495,19.5);
#1230=CIRCLE('',#18496,19.25);
#1231=CIRCLE('',#18498,0.249999999999996);
#1232=CIRCLE('',#18500,0.250000000000004);
#1233=CIRCLE('',#18501,0.250000000000006);
#1234=CIRCLE('',#18503,0.250000000000004);
#1235=CIRCLE('',#18504,0.250000000000004);
#1236=CIRCLE('',#18507,18.1406575306034);
#1237=CIRCLE('',#18508,0.250000000000003);
#1238=CIRCLE('',#18512,0.250000000000004);
#1239=CIRCLE('',#18514,19.25);
#1240=CIRCLE('',#18515,19.5);
#1241=CIRCLE('',#18516,19.5);
#1242=CIRCLE('',#18518,0.250000000000004);
#1243=CIRCLE('',#18519,0.25);
#1244=CIRCLE('',#18521,17.759705149651);
#1245=CIRCLE('',#18522,17.5098863583366);
#1246=CIRCLE('',#18524,19.5);
#1247=CIRCLE('',#18525,19.25);
#1248=CIRCLE('',#18529,0.250000000000004);
#1249=CIRCLE('',#18531,31.5);
#1250=CIRCLE('',#18532,0.25);
#1251=CIRCLE('',#18533,31.25);
#1252=CIRCLE('',#18550,18.2999999762315);
#1253=CIRCLE('',#18552,17.5);
#1254=CIRCLE('',#18553,0.8);
#1255=CIRCLE('',#18566,4.);
#1256=CIRCLE('',#18567,4.);
#1257=CIRCLE('',#18569,4.);
#1258=CIRCLE('',#18570,4.);
#1259=CIRCLE('',#18572,4.);
#1260=CIRCLE('',#18573,4.);
#1261=CIRCLE('',#18575,4.);
#1262=CIRCLE('',#18576,4.);
#1263=CIRCLE('',#18578,4.);
#1264=CIRCLE('',#18579,4.);
#1265=CIRCLE('',#18581,4.);
#1266=CIRCLE('',#18582,4.);
#1267=CIRCLE('',#18584,1.6);
#1268=CIRCLE('',#18585,1.6);
#1269=CIRCLE('',#18586,2.69999999999999);
#1270=CIRCLE('',#18588,1.6);
#1271=CIRCLE('',#18589,1.6);
#1272=CIRCLE('',#18590,2.69999999999999);
#1273=CIRCLE('',#18592,1.6);
#1274=CIRCLE('',#18593,1.6);
#1275=CIRCLE('',#18594,2.7);
#1276=CIRCLE('',#18596,1.6);
#1277=CIRCLE('',#18597,1.6);
#1278=CIRCLE('',#18598,2.7);
#1279=CIRCLE('',#18600,1.6);
#1280=CIRCLE('',#18601,1.6);
#1281=CIRCLE('',#18602,2.69999999999999);
#1282=CIRCLE('',#18604,1.6);
#1283=CIRCLE('',#18605,1.6);
#1284=CIRCLE('',#18606,2.69999999999995);
#1285=CIRCLE('',#18608,1.6);
#1286=CIRCLE('',#18609,1.6);
#1287=CIRCLE('',#18610,2.7);
#1288=CIRCLE('',#18612,1.6);
#1289=CIRCLE('',#18613,1.6);
#1290=CIRCLE('',#18614,2.69999999999995);
#1291=CIRCLE('',#18616,1.6);
#1292=CIRCLE('',#18617,1.6);
#1293=CIRCLE('',#18618,2.69999999999995);
#1294=CIRCLE('',#18620,2.1);
#1295=CIRCLE('',#18621,2.1);
#1296=CIRCLE('',#18622,3.19999999999996);
#1297=CIRCLE('',#18624,1.6);
#1298=CIRCLE('',#18625,1.6);
#1299=CIRCLE('',#18626,2.7);
#1300=CIRCLE('',#18628,1.6);
#1301=CIRCLE('',#18629,1.6);
#1302=CIRCLE('',#18630,2.7);
#1303=CIRCLE('',#18632,1.6);
#1304=CIRCLE('',#18633,1.6);
#1305=CIRCLE('',#18634,2.69999999999999);
#1306=CIRCLE('',#18637,0.800000000000002);
#1307=CIRCLE('',#18638,0.800000000000002);
#1308=CIRCLE('',#18639,0.800000000000002);
#1309=CIRCLE('',#18645,0.800000000000002);
#1310=CIRCLE('',#18647,0.800000000000002);
#1311=CIRCLE('',#18649,0.800000000000002);
#1312=CIRCLE('',#18650,0.799999999999995);
#1313=CIRCLE('',#18652,0.800000000000002);
#1314=CIRCLE('',#18662,1.6);
#1315=CIRCLE('',#18664,1.15469920262284);
#1316=CIRCLE('',#18665,1.15469920262284);
#1317=CIRCLE('',#18667,1.6);
#1318=CIRCLE('',#18669,1.6);
#1319=CIRCLE('',#18671,1.6);
#1320=CIRCLE('',#18673,1.33321558059984);
#1321=CIRCLE('',#18674,1.33321558059984);
#1322=CIRCLE('',#18676,1.32106757713908);
#1323=CIRCLE('',#18677,1.32106757713908);
#1324=CIRCLE('',#18679,2.1);
#1325=CIRCLE('',#18681,1.6);
#1326=CIRCLE('',#18683,1.6);
#1327=CIRCLE('',#18685,1.6);
#1328=CIRCLE('',#18687,1.6);
#1329=CIRCLE('',#18689,1.6);
#1330=CIRCLE('',#18691,1.6);
#1331=CIRCLE('',#18693,1.6);
#1332=CIRCLE('',#18695,1.6);
#1333=CIRCLE('',#18701,7.25609345692882);
#1334=CIRCLE('',#18702,7.25609345692882);
#1335=CIRCLE('',#18706,8.3116573007006);
#1336=CIRCLE('',#18707,8.3116573007006);
#1337=CIRCLE('',#18710,7.62932104676364);
#1338=CIRCLE('',#18711,7.62932104676364);
#1339=CIRCLE('',#18728,0.233315989528693);
#1340=CIRCLE('',#18729,0.233315989528693);
#1341=CIRCLE('',#18731,41.9475849136215);
#1342=CIRCLE('',#18732,41.9475849136215);
#1343=CIRCLE('',#18734,1.);
#1344=CIRCLE('',#18735,1.);
#1345=CIRCLE('',#18736,2.);
#1346=CIRCLE('',#18737,2.);
#1347=CIRCLE('',#18738,1.);
#1348=CIRCLE('',#18739,1.);
#1349=CIRCLE('',#18740,2.);
#1350=CIRCLE('',#18741,2.);
#1351=CIRCLE('',#18744,2.);
#1352=CIRCLE('',#18747,2.);
#1353=CIRCLE('',#18759,0.399999999999998);
#1354=CIRCLE('',#18760,0.400000000000011);
#1355=CIRCLE('',#18762,0.399999999999998);
#1356=CIRCLE('',#18763,0.400000000000011);
#1357=CIRCLE('',#18765,0.400000000000011);
#1358=CIRCLE('',#18766,0.399999999999998);
#1359=CIRCLE('',#18768,0.400000000000011);
#1360=CIRCLE('',#18769,0.399999999999998);
#1361=CIRCLE('',#18789,1.60000000000001);
#1362=CIRCLE('',#18808,1.60000000000001);
#1363=CIRCLE('',#18810,1.60000000000001);
#1364=CIRCLE('',#18833,8.50000000000001);
#1365=CIRCLE('',#18845,8.1);
#1366=CIRCLE('',#18851,12.);
#1367=CIRCLE('',#18856,12.);
#1368=CIRCLE('',#18861,12.);
#1369=CIRCLE('',#18866,12.);
#1370=CIRCLE('',#18867,12.);
#1371=CIRCLE('',#18872,14.);
#1372=CIRCLE('',#18873,14.);
#1373=CIRCLE('',#18875,12.);
#1374=CIRCLE('',#18877,12.);
#1375=CIRCLE('',#18878,12.);
#1376=CIRCLE('',#18879,12.);
#1377=CIRCLE('',#18880,12.);
#1378=CIRCLE('',#18883,8.1);
#1379=CIRCLE('',#18884,8.1);
#1380=CIRCLE('',#18886,11.2187458390495);
#1381=CIRCLE('',#18887,4.22441061393973);
#1382=CIRCLE('',#18889,14.);
#1383=CIRCLE('',#18890,14.);
#1384=CIRCLE('',#18891,14.);
#1385=CIRCLE('',#18893,14.);
#1386=CIRCLE('',#18895,14.);
#1387=CIRCLE('',#18897,14.);
#1388=CIRCLE('',#18903,6.29999999999999);
#1389=CIRCLE('',#18905,6.00000000000001);
#1390=CIRCLE('',#18906,6.00000000000001);
#1391=CIRCLE('',#18908,8.49999999999999);
#1392=CIRCLE('',#18912,0.3);
#1393=CIRCLE('',#18914,9.7);
#1394=CIRCLE('',#18915,0.3);
#1395=CIRCLE('',#18916,10.);
#1396=CIRCLE('',#18917,10.);
#1397=CIRCLE('',#18919,4.75);
#1398=CIRCLE('',#18920,4.75);
#1399=CIRCLE('',#18922,7.00000000000001);
#1400=CIRCLE('',#18923,7.00000000000001);
#1401=CIRCLE('',#18926,6.00000000000001);
#1402=CIRCLE('',#18928,10.);
#1403=CIRCLE('',#18929,10.);
#1404=CIRCLE('',#18930,10.);
#1405=CIRCLE('',#18931,10.);
#1406=CIRCLE('',#18932,10.);
#1407=CIRCLE('',#18933,10.);
#1408=CIRCLE('',#18934,10.);
#1409=CIRCLE('',#18935,10.);
#1410=CIRCLE('',#18936,10.);
#1411=CIRCLE('',#18938,8.49999999999999);
#1412=CIRCLE('',#18940,1.2500000000005);
#1413=CIRCLE('',#18941,1.2500000000005);
#1414=CIRCLE('',#18943,1.25000000000059);
#1415=CIRCLE('',#18945,1.25000000000024);
#1416=CIRCLE('',#18947,1.24999999999999);
#1417=CIRCLE('',#18949,1.2500000000005);
#1418=CIRCLE('',#18950,1.2500000000005);
#1419=CIRCLE('',#18952,1.25000000000059);
#1420=CIRCLE('',#18953,1.25000000000059);
#1421=CIRCLE('',#18954,1.25000000000059);
#1422=CIRCLE('',#18956,1.25000000000024);
#1423=CIRCLE('',#18957,1.25000000000024);
#1424=CIRCLE('',#18958,1.25000000000024);
#1425=CIRCLE('',#18960,1.24999999999999);
#1426=CIRCLE('',#18961,1.24999999999999);
#1427=CIRCLE('',#18962,1.24999999999999);
#1428=CIRCLE('',#18964,6.00000000000001);
#1429=CIRCLE('',#19059,4.);
#1430=CIRCLE('',#19061,4.);
#1431=CIRCLE('',#19063,3.99999999999999);
#1432=CIRCLE('',#19064,3.99999999999999);
#1433=CIRCLE('',#19069,1.60000000000001);
#1434=CIRCLE('',#19071,1.60000000000001);
#1435=CIRCLE('',#19073,2.);
#1436=CIRCLE('',#19075,2.);
#1437=CIRCLE('',#19077,3.6);
#1438=CIRCLE('',#19079,3.99999999999999);
#1439=CIRCLE('',#19080,3.6);
#1440=CIRCLE('',#19088,1.4);
#1441=CIRCLE('',#19090,1.4);
#1442=CIRCLE('',#19091,1.4);
#1443=CIRCLE('',#19094,1.4);
#1444=CIRCLE('',#19118,1.6);
#1445=CIRCLE('',#19120,1.6);
#1446=CIRCLE('',#19122,1.6);
#1447=CIRCLE('',#19124,1.6);
#1448=CIRCLE('',#19132,2.);
#1449=CIRCLE('',#19133,2.);
#1450=CIRCLE('',#19135,2.);
#1451=CIRCLE('',#19136,2.);
#1452=CIRCLE('',#19144,1.6);
#1453=CIRCLE('',#19146,1.6);
#1454=CIRCLE('',#19148,1.6);
#1455=CIRCLE('',#19150,1.6);
#1456=CIRCLE('',#19170,4.);
#1457=CIRCLE('',#19171,3.6);
#1458=CIRCLE('',#19173,4.);
#1459=CIRCLE('',#19174,4.);
#1460=CIRCLE('',#19177,1.6);
#1461=CIRCLE('',#19191,1.6);
#1462=CIRCLE('',#19207,1.60000000000001);
#1463=CIRCLE('',#19208,1.6);
#1464=CIRCLE('',#19210,1.49172584788676);
#1465=CIRCLE('',#19211,1.49172584788676);
#1466=CIRCLE('',#19213,1.04190416256385);
#1467=CIRCLE('',#19214,1.04190416256385);
#1468=CIRCLE('',#19216,11.8);
#1469=CIRCLE('',#19217,0.2);
#1470=CIRCLE('',#19218,12.);
#1471=CIRCLE('',#19219,12.);
#1472=CIRCLE('',#19221,12.);
#1473=CIRCLE('',#19222,12.);
#1474=CIRCLE('',#19223,0.2);
#1475=CIRCLE('',#19224,11.8);
#1476=CIRCLE('',#19226,3.25);
#1477=CIRCLE('',#19227,3.25);
#1478=CIRCLE('',#19228,0.2);
#1479=CIRCLE('',#19229,3.45);
#1480=CIRCLE('',#19231,3.45);
#1481=CIRCLE('',#19232,0.2);
#1482=CIRCLE('',#19233,3.25);
#1483=CIRCLE('',#19234,3.25);
#1484=CIRCLE('',#19239,7.);
#1485=CIRCLE('',#19241,2.);
#1486=CIRCLE('',#19243,1.6);
#1487=CIRCLE('',#19244,1.6);
#1488=CIRCLE('',#19249,1.6);
#1489=CIRCLE('',#19251,2.);
#1490=CIRCLE('',#19254,4.);
#1491=CIRCLE('',#19255,4.);
#1492=CIRCLE('',#19256,3.6);
#1493=CIRCLE('',#19261,5.);
#1494=CIRCLE('',#19262,0.5);
#1495=CIRCLE('',#19263,4.5);
#1496=CIRCLE('',#19265,4.5);
#1497=CIRCLE('',#19266,0.5);
#1498=CIRCLE('',#19267,5.);
#1499=CIRCLE('',#19270,7.);
#1500=CIRCLE('',#19272,4.22087352428905);
#1501=CIRCLE('',#19273,4.22087352428905);
#1502=CIRCLE('',#19275,1.6);
#1503=CIRCLE('',#19276,1.6);
#1504=CIRCLE('',#19278,5.14310210370206);
#1505=CIRCLE('',#19280,4.5);
#1506=CIRCLE('',#19281,4.5);
#1507=CIRCLE('',#19283,5.14310210370206);
#1508=CIRCLE('',#19284,4.);
#1509=CIRCLE('',#19286,0.599999999999998);
#1510=CIRCLE('',#19287,0.599999999999998);
#1511=CIRCLE('',#19288,0.599999999999998);
#1512=CIRCLE('',#19289,0.599999999999998);
#1513=CIRCLE('',#19352,1.60000000000001);
#1514=CIRCLE('',#19354,1.6);
#1515=CIRCLE('',#19357,4.50000000000007);
#1516=CIRCLE('',#19358,4.50000000000007);
#1517=CIRCLE('',#19398,4.11168229960152);
#1518=CIRCLE('',#19399,4.11168229960152);
#1519=CIRCLE('',#19407,1.49172584788676);
#1520=CIRCLE('',#19408,1.49172584788676);
#1521=CIRCLE('',#19411,4.6918515041613);
#1522=CIRCLE('',#19412,4.6918515041613);
#1523=CIRCLE('',#19418,0.338583852498097);
#1524=CIRCLE('',#19419,0.338583852498097);
#1525=CIRCLE('',#19424,2.81299719163292);
#1526=CIRCLE('',#19425,2.81299719163292);
#1527=FACE_OUTER_BOUND('',#2458,.T.);
#1528=FACE_OUTER_BOUND('',#2511,.T.);
#1529=FACE_OUTER_BOUND('',#2564,.T.);
#1530=FACE_OUTER_BOUND('',#2565,.T.);
#1531=FACE_OUTER_BOUND('',#2566,.T.);
#1532=FACE_OUTER_BOUND('',#2567,.T.);
#1533=FACE_OUTER_BOUND('',#2568,.T.);
#1534=FACE_OUTER_BOUND('',#2569,.T.);
#1535=FACE_OUTER_BOUND('',#2570,.T.);
#1536=FACE_OUTER_BOUND('',#2571,.T.);
#1537=FACE_OUTER_BOUND('',#2572,.T.);
#1538=FACE_OUTER_BOUND('',#2573,.T.);
#1539=FACE_OUTER_BOUND('',#2574,.T.);
#1540=FACE_OUTER_BOUND('',#2575,.T.);
#1541=FACE_OUTER_BOUND('',#2576,.T.);
#1542=FACE_OUTER_BOUND('',#2577,.T.);
#1543=FACE_OUTER_BOUND('',#2578,.T.);
#1544=FACE_OUTER_BOUND('',#2579,.T.);
#1545=FACE_OUTER_BOUND('',#2580,.T.);
#1546=FACE_OUTER_BOUND('',#2581,.T.);
#1547=FACE_OUTER_BOUND('',#2582,.T.);
#1548=FACE_OUTER_BOUND('',#2583,.T.);
#1549=FACE_OUTER_BOUND('',#2584,.T.);
#1550=FACE_OUTER_BOUND('',#2585,.T.);
#1551=FACE_OUTER_BOUND('',#2586,.T.);
#1552=FACE_OUTER_BOUND('',#2587,.T.);
#1553=FACE_OUTER_BOUND('',#2588,.T.);
#1554=FACE_OUTER_BOUND('',#2589,.T.);
#1555=FACE_OUTER_BOUND('',#2590,.T.);
#1556=FACE_OUTER_BOUND('',#2591,.T.);
#1557=FACE_OUTER_BOUND('',#2592,.T.);
#1558=FACE_OUTER_BOUND('',#2593,.T.);
#1559=FACE_OUTER_BOUND('',#2594,.T.);
#1560=FACE_OUTER_BOUND('',#2595,.T.);
#1561=FACE_OUTER_BOUND('',#2596,.T.);
#1562=FACE_OUTER_BOUND('',#2597,.T.);
#1563=FACE_OUTER_BOUND('',#2598,.T.);
#1564=FACE_OUTER_BOUND('',#2599,.T.);
#1565=FACE_OUTER_BOUND('',#2600,.T.);
#1566=FACE_OUTER_BOUND('',#2601,.T.);
#1567=FACE_OUTER_BOUND('',#2602,.T.);
#1568=FACE_OUTER_BOUND('',#2603,.T.);
#1569=FACE_OUTER_BOUND('',#2604,.T.);
#1570=FACE_OUTER_BOUND('',#2605,.T.);
#1571=FACE_OUTER_BOUND('',#2606,.T.);
#1572=FACE_OUTER_BOUND('',#2607,.T.);
#1573=FACE_OUTER_BOUND('',#2608,.T.);
#1574=FACE_OUTER_BOUND('',#2609,.T.);
#1575=FACE_OUTER_BOUND('',#2610,.T.);
#1576=FACE_OUTER_BOUND('',#2611,.T.);
#1577=FACE_OUTER_BOUND('',#2612,.T.);
#1578=FACE_OUTER_BOUND('',#2613,.T.);
#1579=FACE_OUTER_BOUND('',#2614,.T.);
#1580=FACE_OUTER_BOUND('',#2615,.T.);
#1581=FACE_OUTER_BOUND('',#2616,.T.);
#1582=FACE_OUTER_BOUND('',#2617,.T.);
#1583=FACE_OUTER_BOUND('',#2618,.T.);
#1584=FACE_OUTER_BOUND('',#2619,.T.);
#1585=FACE_OUTER_BOUND('',#2620,.T.);
#1586=FACE_OUTER_BOUND('',#2621,.T.);
#1587=FACE_OUTER_BOUND('',#2622,.T.);
#1588=FACE_OUTER_BOUND('',#2623,.T.);
#1589=FACE_OUTER_BOUND('',#2624,.T.);
#1590=FACE_OUTER_BOUND('',#2625,.T.);
#1591=FACE_OUTER_BOUND('',#2626,.T.);
#1592=FACE_OUTER_BOUND('',#2627,.T.);
#1593=FACE_OUTER_BOUND('',#2628,.T.);
#1594=FACE_OUTER_BOUND('',#2629,.T.);
#1595=FACE_OUTER_BOUND('',#2630,.T.);
#1596=FACE_OUTER_BOUND('',#2631,.T.);
#1597=FACE_OUTER_BOUND('',#2632,.T.);
#1598=FACE_OUTER_BOUND('',#2633,.T.);
#1599=FACE_OUTER_BOUND('',#2634,.T.);
#1600=FACE_OUTER_BOUND('',#2635,.T.);
#1601=FACE_OUTER_BOUND('',#2636,.T.);
#1602=FACE_OUTER_BOUND('',#2637,.T.);
#1603=FACE_OUTER_BOUND('',#2638,.T.);
#1604=FACE_OUTER_BOUND('',#2639,.T.);
#1605=FACE_OUTER_BOUND('',#2640,.T.);
#1606=FACE_OUTER_BOUND('',#2641,.T.);
#1607=FACE_OUTER_BOUND('',#2642,.T.);
#1608=FACE_OUTER_BOUND('',#2643,.T.);
#1609=FACE_OUTER_BOUND('',#2644,.T.);
#1610=FACE_OUTER_BOUND('',#2645,.T.);
#1611=FACE_OUTER_BOUND('',#2646,.T.);
#1612=FACE_OUTER_BOUND('',#2647,.T.);
#1613=FACE_OUTER_BOUND('',#2648,.T.);
#1614=FACE_OUTER_BOUND('',#2649,.T.);
#1615=FACE_OUTER_BOUND('',#2650,.T.);
#1616=FACE_OUTER_BOUND('',#2651,.T.);
#1617=FACE_OUTER_BOUND('',#2652,.T.);
#1618=FACE_OUTER_BOUND('',#2653,.T.);
#1619=FACE_OUTER_BOUND('',#2654,.T.);
#1620=FACE_OUTER_BOUND('',#2655,.T.);
#1621=FACE_OUTER_BOUND('',#2656,.T.);
#1622=FACE_OUTER_BOUND('',#2657,.T.);
#1623=FACE_OUTER_BOUND('',#2658,.T.);
#1624=FACE_OUTER_BOUND('',#2659,.T.);
#1625=FACE_OUTER_BOUND('',#2660,.T.);
#1626=FACE_OUTER_BOUND('',#2661,.T.);
#1627=FACE_OUTER_BOUND('',#2662,.T.);
#1628=FACE_OUTER_BOUND('',#2663,.T.);
#1629=FACE_OUTER_BOUND('',#2664,.T.);
#1630=FACE_OUTER_BOUND('',#2665,.T.);
#1631=FACE_OUTER_BOUND('',#2666,.T.);
#1632=FACE_OUTER_BOUND('',#2667,.T.);
#1633=FACE_OUTER_BOUND('',#2668,.T.);
#1634=FACE_OUTER_BOUND('',#2669,.T.);
#1635=FACE_OUTER_BOUND('',#2670,.T.);
#1636=FACE_OUTER_BOUND('',#2671,.T.);
#1637=FACE_OUTER_BOUND('',#2672,.T.);
#1638=FACE_OUTER_BOUND('',#2673,.T.);
#1639=FACE_OUTER_BOUND('',#2674,.T.);
#1640=FACE_OUTER_BOUND('',#2675,.T.);
#1641=FACE_OUTER_BOUND('',#2676,.T.);
#1642=FACE_OUTER_BOUND('',#2677,.T.);
#1643=FACE_OUTER_BOUND('',#2678,.T.);
#1644=FACE_OUTER_BOUND('',#2679,.T.);
#1645=FACE_OUTER_BOUND('',#2680,.T.);
#1646=FACE_OUTER_BOUND('',#2681,.T.);
#1647=FACE_OUTER_BOUND('',#2682,.T.);
#1648=FACE_OUTER_BOUND('',#2683,.T.);
#1649=FACE_OUTER_BOUND('',#2684,.T.);
#1650=FACE_OUTER_BOUND('',#2685,.T.);
#1651=FACE_OUTER_BOUND('',#2686,.T.);
#1652=FACE_OUTER_BOUND('',#2687,.T.);
#1653=FACE_OUTER_BOUND('',#2688,.T.);
#1654=FACE_OUTER_BOUND('',#2689,.T.);
#1655=FACE_OUTER_BOUND('',#2690,.T.);
#1656=FACE_OUTER_BOUND('',#2691,.T.);
#1657=FACE_OUTER_BOUND('',#2692,.T.);
#1658=FACE_OUTER_BOUND('',#2693,.T.);
#1659=FACE_OUTER_BOUND('',#2694,.T.);
#1660=FACE_OUTER_BOUND('',#2695,.T.);
#1661=FACE_OUTER_BOUND('',#2696,.T.);
#1662=FACE_OUTER_BOUND('',#2697,.T.);
#1663=FACE_OUTER_BOUND('',#2698,.T.);
#1664=FACE_OUTER_BOUND('',#2699,.T.);
#1665=FACE_OUTER_BOUND('',#2700,.T.);
#1666=FACE_OUTER_BOUND('',#2701,.T.);
#1667=FACE_OUTER_BOUND('',#2702,.T.);
#1668=FACE_OUTER_BOUND('',#2703,.T.);
#1669=FACE_OUTER_BOUND('',#2704,.T.);
#1670=FACE_OUTER_BOUND('',#2705,.T.);
#1671=FACE_OUTER_BOUND('',#2706,.T.);
#1672=FACE_OUTER_BOUND('',#2707,.T.);
#1673=FACE_OUTER_BOUND('',#2708,.T.);
#1674=FACE_OUTER_BOUND('',#2709,.T.);
#1675=FACE_OUTER_BOUND('',#2710,.T.);
#1676=FACE_OUTER_BOUND('',#2711,.T.);
#1677=FACE_OUTER_BOUND('',#2712,.T.);
#1678=FACE_OUTER_BOUND('',#2713,.T.);
#1679=FACE_OUTER_BOUND('',#2714,.T.);
#1680=FACE_OUTER_BOUND('',#2715,.T.);
#1681=FACE_OUTER_BOUND('',#2716,.T.);
#1682=FACE_OUTER_BOUND('',#2717,.T.);
#1683=FACE_OUTER_BOUND('',#2718,.T.);
#1684=FACE_OUTER_BOUND('',#2719,.T.);
#1685=FACE_OUTER_BOUND('',#2720,.T.);
#1686=FACE_OUTER_BOUND('',#2721,.T.);
#1687=FACE_OUTER_BOUND('',#2722,.T.);
#1688=FACE_OUTER_BOUND('',#2723,.T.);
#1689=FACE_OUTER_BOUND('',#2724,.T.);
#1690=FACE_OUTER_BOUND('',#2726,.T.);
#1691=FACE_OUTER_BOUND('',#2727,.T.);
#1692=FACE_OUTER_BOUND('',#2728,.T.);
#1693=FACE_OUTER_BOUND('',#2729,.T.);
#1694=FACE_OUTER_BOUND('',#2730,.T.);
#1695=FACE_OUTER_BOUND('',#2731,.T.);
#1696=FACE_OUTER_BOUND('',#2732,.T.);
#1697=FACE_OUTER_BOUND('',#2733,.T.);
#1698=FACE_OUTER_BOUND('',#2734,.T.);
#1699=FACE_OUTER_BOUND('',#2735,.T.);
#1700=FACE_OUTER_BOUND('',#2736,.T.);
#1701=FACE_OUTER_BOUND('',#2737,.T.);
#1702=FACE_OUTER_BOUND('',#2738,.T.);
#1703=FACE_OUTER_BOUND('',#2739,.T.);
#1704=FACE_OUTER_BOUND('',#2740,.T.);
#1705=FACE_OUTER_BOUND('',#2741,.T.);
#1706=FACE_OUTER_BOUND('',#2742,.T.);
#1707=FACE_OUTER_BOUND('',#2743,.T.);
#1708=FACE_OUTER_BOUND('',#2744,.T.);
#1709=FACE_OUTER_BOUND('',#2745,.T.);
#1710=FACE_OUTER_BOUND('',#2746,.T.);
#1711=FACE_OUTER_BOUND('',#2747,.T.);
#1712=FACE_OUTER_BOUND('',#2748,.T.);
#1713=FACE_OUTER_BOUND('',#2749,.T.);
#1714=FACE_OUTER_BOUND('',#2750,.T.);
#1715=FACE_OUTER_BOUND('',#2751,.T.);
#1716=FACE_OUTER_BOUND('',#2752,.T.);
#1717=FACE_OUTER_BOUND('',#2753,.T.);
#1718=FACE_OUTER_BOUND('',#2754,.T.);
#1719=FACE_OUTER_BOUND('',#2755,.T.);
#1720=FACE_OUTER_BOUND('',#2756,.T.);
#1721=FACE_OUTER_BOUND('',#2757,.T.);
#1722=FACE_OUTER_BOUND('',#2758,.T.);
#1723=FACE_OUTER_BOUND('',#2759,.T.);
#1724=FACE_OUTER_BOUND('',#2760,.T.);
#1725=FACE_OUTER_BOUND('',#2761,.T.);
#1726=FACE_OUTER_BOUND('',#2762,.T.);
#1727=FACE_OUTER_BOUND('',#2763,.T.);
#1728=FACE_OUTER_BOUND('',#2764,.T.);
#1729=FACE_OUTER_BOUND('',#2765,.T.);
#1730=FACE_OUTER_BOUND('',#2766,.T.);
#1731=FACE_OUTER_BOUND('',#2767,.T.);
#1732=FACE_OUTER_BOUND('',#2768,.T.);
#1733=FACE_OUTER_BOUND('',#2769,.T.);
#1734=FACE_OUTER_BOUND('',#2770,.T.);
#1735=FACE_OUTER_BOUND('',#2771,.T.);
#1736=FACE_OUTER_BOUND('',#2772,.T.);
#1737=FACE_OUTER_BOUND('',#2773,.T.);
#1738=FACE_OUTER_BOUND('',#2774,.T.);
#1739=FACE_OUTER_BOUND('',#2775,.T.);
#1740=FACE_OUTER_BOUND('',#2776,.T.);
#1741=FACE_OUTER_BOUND('',#2777,.T.);
#1742=FACE_OUTER_BOUND('',#2778,.T.);
#1743=FACE_OUTER_BOUND('',#2779,.T.);
#1744=FACE_OUTER_BOUND('',#2782,.T.);
#1745=FACE_OUTER_BOUND('',#2783,.T.);
#1746=FACE_OUTER_BOUND('',#2784,.T.);
#1747=FACE_OUTER_BOUND('',#2785,.T.);
#1748=FACE_OUTER_BOUND('',#2786,.T.);
#1749=FACE_OUTER_BOUND('',#2787,.T.);
#1750=FACE_OUTER_BOUND('',#2790,.T.);
#1751=FACE_OUTER_BOUND('',#2791,.T.);
#1752=FACE_OUTER_BOUND('',#2792,.T.);
#1753=FACE_OUTER_BOUND('',#2793,.T.);
#1754=FACE_OUTER_BOUND('',#2794,.T.);
#1755=FACE_OUTER_BOUND('',#2795,.T.);
#1756=FACE_OUTER_BOUND('',#2796,.T.);
#1757=FACE_OUTER_BOUND('',#2797,.T.);
#1758=FACE_OUTER_BOUND('',#2798,.T.);
#1759=FACE_OUTER_BOUND('',#2799,.T.);
#1760=FACE_OUTER_BOUND('',#2800,.T.);
#1761=FACE_OUTER_BOUND('',#2801,.T.);
#1762=FACE_OUTER_BOUND('',#2802,.T.);
#1763=FACE_OUTER_BOUND('',#2803,.T.);
#1764=FACE_OUTER_BOUND('',#2804,.T.);
#1765=FACE_OUTER_BOUND('',#2805,.T.);
#1766=FACE_OUTER_BOUND('',#2806,.T.);
#1767=FACE_OUTER_BOUND('',#2807,.T.);
#1768=FACE_OUTER_BOUND('',#2808,.T.);
#1769=FACE_OUTER_BOUND('',#2809,.T.);
#1770=FACE_OUTER_BOUND('',#2810,.T.);
#1771=FACE_OUTER_BOUND('',#2811,.T.);
#1772=FACE_OUTER_BOUND('',#2812,.T.);
#1773=FACE_OUTER_BOUND('',#2813,.T.);
#1774=FACE_OUTER_BOUND('',#2814,.T.);
#1775=FACE_OUTER_BOUND('',#2815,.T.);
#1776=FACE_OUTER_BOUND('',#2816,.T.);
#1777=FACE_OUTER_BOUND('',#2817,.T.);
#1778=FACE_OUTER_BOUND('',#2818,.T.);
#1779=FACE_OUTER_BOUND('',#2819,.T.);
#1780=FACE_OUTER_BOUND('',#2820,.T.);
#1781=FACE_OUTER_BOUND('',#2821,.T.);
#1782=FACE_OUTER_BOUND('',#2823,.T.);
#1783=FACE_OUTER_BOUND('',#2824,.T.);
#1784=FACE_OUTER_BOUND('',#2826,.T.);
#1785=FACE_OUTER_BOUND('',#2827,.T.);
#1786=FACE_OUTER_BOUND('',#2829,.T.);
#1787=FACE_OUTER_BOUND('',#2830,.T.);
#1788=FACE_OUTER_BOUND('',#2831,.T.);
#1789=FACE_OUTER_BOUND('',#2833,.T.);
#1790=FACE_OUTER_BOUND('',#2834,.T.);
#1791=FACE_OUTER_BOUND('',#2835,.T.);
#1792=FACE_OUTER_BOUND('',#2836,.T.);
#1793=FACE_OUTER_BOUND('',#2837,.T.);
#1794=FACE_OUTER_BOUND('',#2838,.T.);
#1795=FACE_OUTER_BOUND('',#2839,.T.);
#1796=FACE_OUTER_BOUND('',#2840,.T.);
#1797=FACE_OUTER_BOUND('',#2841,.T.);
#1798=FACE_OUTER_BOUND('',#2842,.T.);
#1799=FACE_OUTER_BOUND('',#2843,.T.);
#1800=FACE_OUTER_BOUND('',#2844,.T.);
#1801=FACE_OUTER_BOUND('',#2845,.T.);
#1802=FACE_OUTER_BOUND('',#2846,.T.);
#1803=FACE_OUTER_BOUND('',#2847,.T.);
#1804=FACE_OUTER_BOUND('',#2848,.T.);
#1805=FACE_OUTER_BOUND('',#2849,.T.);
#1806=FACE_OUTER_BOUND('',#2850,.T.);
#1807=FACE_OUTER_BOUND('',#2851,.T.);
#1808=FACE_OUTER_BOUND('',#2852,.T.);
#1809=FACE_OUTER_BOUND('',#2853,.T.);
#1810=FACE_OUTER_BOUND('',#2854,.T.);
#1811=FACE_OUTER_BOUND('',#2855,.T.);
#1812=FACE_OUTER_BOUND('',#2856,.T.);
#1813=FACE_OUTER_BOUND('',#2857,.T.);
#1814=FACE_OUTER_BOUND('',#2858,.T.);
#1815=FACE_OUTER_BOUND('',#2859,.T.);
#1816=FACE_OUTER_BOUND('',#2860,.T.);
#1817=FACE_OUTER_BOUND('',#2861,.T.);
#1818=FACE_OUTER_BOUND('',#2862,.T.);
#1819=FACE_OUTER_BOUND('',#2863,.T.);
#1820=FACE_OUTER_BOUND('',#2864,.T.);
#1821=FACE_OUTER_BOUND('',#2865,.T.);
#1822=FACE_OUTER_BOUND('',#2866,.T.);
#1823=FACE_OUTER_BOUND('',#2867,.T.);
#1824=FACE_OUTER_BOUND('',#2868,.T.);
#1825=FACE_OUTER_BOUND('',#2869,.T.);
#1826=FACE_OUTER_BOUND('',#2870,.T.);
#1827=FACE_OUTER_BOUND('',#2871,.T.);
#1828=FACE_OUTER_BOUND('',#2872,.T.);
#1829=FACE_OUTER_BOUND('',#2873,.T.);
#1830=FACE_OUTER_BOUND('',#2874,.T.);
#1831=FACE_OUTER_BOUND('',#2875,.T.);
#1832=FACE_OUTER_BOUND('',#2876,.T.);
#1833=FACE_OUTER_BOUND('',#2877,.T.);
#1834=FACE_OUTER_BOUND('',#2878,.T.);
#1835=FACE_OUTER_BOUND('',#2879,.T.);
#1836=FACE_OUTER_BOUND('',#2880,.T.);
#1837=FACE_OUTER_BOUND('',#2881,.T.);
#1838=FACE_OUTER_BOUND('',#2882,.T.);
#1839=FACE_OUTER_BOUND('',#2883,.T.);
#1840=FACE_OUTER_BOUND('',#2884,.T.);
#1841=FACE_OUTER_BOUND('',#2885,.T.);
#1842=FACE_OUTER_BOUND('',#2886,.T.);
#1843=FACE_OUTER_BOUND('',#2887,.T.);
#1844=FACE_OUTER_BOUND('',#2888,.T.);
#1845=FACE_OUTER_BOUND('',#2889,.T.);
#1846=FACE_OUTER_BOUND('',#2890,.T.);
#1847=FACE_OUTER_BOUND('',#2891,.T.);
#1848=FACE_OUTER_BOUND('',#2892,.T.);
#1849=FACE_OUTER_BOUND('',#2893,.T.);
#1850=FACE_OUTER_BOUND('',#2894,.T.);
#1851=FACE_OUTER_BOUND('',#2895,.T.);
#1852=FACE_OUTER_BOUND('',#2896,.T.);
#1853=FACE_OUTER_BOUND('',#2897,.T.);
#1854=FACE_OUTER_BOUND('',#2898,.T.);
#1855=FACE_OUTER_BOUND('',#2899,.T.);
#1856=FACE_OUTER_BOUND('',#2900,.T.);
#1857=FACE_OUTER_BOUND('',#2901,.T.);
#1858=FACE_OUTER_BOUND('',#2902,.T.);
#1859=FACE_OUTER_BOUND('',#2903,.T.);
#1860=FACE_OUTER_BOUND('',#2904,.T.);
#1861=FACE_OUTER_BOUND('',#2905,.T.);
#1862=FACE_OUTER_BOUND('',#2906,.T.);
#1863=FACE_OUTER_BOUND('',#2907,.T.);
#1864=FACE_OUTER_BOUND('',#2908,.T.);
#1865=FACE_OUTER_BOUND('',#2909,.T.);
#1866=FACE_OUTER_BOUND('',#2910,.T.);
#1867=FACE_OUTER_BOUND('',#2911,.T.);
#1868=FACE_OUTER_BOUND('',#2912,.T.);
#1869=FACE_OUTER_BOUND('',#2914,.T.);
#1870=FACE_OUTER_BOUND('',#2915,.T.);
#1871=FACE_OUTER_BOUND('',#2916,.T.);
#1872=FACE_OUTER_BOUND('',#2917,.T.);
#1873=FACE_OUTER_BOUND('',#2918,.T.);
#1874=FACE_OUTER_BOUND('',#2919,.T.);
#1875=FACE_OUTER_BOUND('',#2921,.T.);
#1876=FACE_OUTER_BOUND('',#2922,.T.);
#1877=FACE_OUTER_BOUND('',#2923,.T.);
#1878=FACE_OUTER_BOUND('',#2924,.T.);
#1879=FACE_OUTER_BOUND('',#2925,.T.);
#1880=FACE_OUTER_BOUND('',#2926,.T.);
#1881=FACE_OUTER_BOUND('',#2927,.T.);
#1882=FACE_OUTER_BOUND('',#2928,.T.);
#1883=FACE_OUTER_BOUND('',#2929,.T.);
#1884=FACE_OUTER_BOUND('',#2930,.T.);
#1885=FACE_OUTER_BOUND('',#2931,.T.);
#1886=FACE_OUTER_BOUND('',#2932,.T.);
#1887=FACE_OUTER_BOUND('',#2933,.T.);
#1888=FACE_OUTER_BOUND('',#2934,.T.);
#1889=FACE_OUTER_BOUND('',#2935,.T.);
#1890=FACE_OUTER_BOUND('',#2936,.T.);
#1891=FACE_OUTER_BOUND('',#2937,.T.);
#1892=FACE_OUTER_BOUND('',#2938,.T.);
#1893=FACE_OUTER_BOUND('',#2939,.T.);
#1894=FACE_OUTER_BOUND('',#2940,.T.);
#1895=FACE_OUTER_BOUND('',#2941,.T.);
#1896=FACE_OUTER_BOUND('',#2942,.T.);
#1897=FACE_OUTER_BOUND('',#2943,.T.);
#1898=FACE_OUTER_BOUND('',#2944,.T.);
#1899=FACE_OUTER_BOUND('',#2945,.T.);
#1900=FACE_OUTER_BOUND('',#2946,.T.);
#1901=FACE_OUTER_BOUND('',#2947,.T.);
#1902=FACE_OUTER_BOUND('',#2948,.T.);
#1903=FACE_OUTER_BOUND('',#2949,.T.);
#1904=FACE_OUTER_BOUND('',#2950,.T.);
#1905=FACE_OUTER_BOUND('',#2951,.T.);
#1906=FACE_OUTER_BOUND('',#2952,.T.);
#1907=FACE_OUTER_BOUND('',#2953,.T.);
#1908=FACE_OUTER_BOUND('',#2954,.T.);
#1909=FACE_OUTER_BOUND('',#2955,.T.);
#1910=FACE_OUTER_BOUND('',#2956,.T.);
#1911=FACE_OUTER_BOUND('',#2957,.T.);
#1912=FACE_OUTER_BOUND('',#2958,.T.);
#1913=FACE_OUTER_BOUND('',#2959,.T.);
#1914=FACE_OUTER_BOUND('',#2960,.T.);
#1915=FACE_OUTER_BOUND('',#2961,.T.);
#1916=FACE_OUTER_BOUND('',#2962,.T.);
#1917=FACE_OUTER_BOUND('',#2963,.T.);
#1918=FACE_OUTER_BOUND('',#2964,.T.);
#1919=FACE_OUTER_BOUND('',#2965,.T.);
#1920=FACE_OUTER_BOUND('',#2966,.T.);
#1921=FACE_OUTER_BOUND('',#2967,.T.);
#1922=FACE_OUTER_BOUND('',#2968,.T.);
#1923=FACE_OUTER_BOUND('',#2969,.T.);
#1924=FACE_OUTER_BOUND('',#2970,.T.);
#1925=FACE_OUTER_BOUND('',#2971,.T.);
#1926=FACE_OUTER_BOUND('',#2972,.T.);
#1927=FACE_OUTER_BOUND('',#2973,.T.);
#1928=FACE_OUTER_BOUND('',#2974,.T.);
#1929=FACE_OUTER_BOUND('',#2975,.T.);
#1930=FACE_OUTER_BOUND('',#2976,.T.);
#1931=FACE_OUTER_BOUND('',#2977,.T.);
#1932=FACE_OUTER_BOUND('',#2978,.T.);
#1933=FACE_OUTER_BOUND('',#2979,.T.);
#1934=FACE_OUTER_BOUND('',#2980,.T.);
#1935=FACE_OUTER_BOUND('',#2981,.T.);
#1936=FACE_OUTER_BOUND('',#2982,.T.);
#1937=FACE_OUTER_BOUND('',#2983,.T.);
#1938=FACE_OUTER_BOUND('',#2984,.T.);
#1939=FACE_OUTER_BOUND('',#2985,.T.);
#1940=FACE_OUTER_BOUND('',#2986,.T.);
#1941=FACE_OUTER_BOUND('',#2987,.T.);
#1942=FACE_OUTER_BOUND('',#2988,.T.);
#1943=FACE_OUTER_BOUND('',#2989,.T.);
#1944=FACE_OUTER_BOUND('',#2990,.T.);
#1945=FACE_OUTER_BOUND('',#2991,.T.);
#1946=FACE_OUTER_BOUND('',#2992,.T.);
#1947=FACE_OUTER_BOUND('',#2993,.T.);
#1948=FACE_OUTER_BOUND('',#2994,.T.);
#1949=FACE_OUTER_BOUND('',#2995,.T.);
#1950=FACE_OUTER_BOUND('',#2996,.T.);
#1951=FACE_OUTER_BOUND('',#2997,.T.);
#1952=FACE_OUTER_BOUND('',#2998,.T.);
#1953=FACE_OUTER_BOUND('',#3016,.T.);
#1954=FACE_OUTER_BOUND('',#3034,.T.);
#1955=FACE_OUTER_BOUND('',#3035,.T.);
#1956=FACE_OUTER_BOUND('',#3036,.T.);
#1957=FACE_OUTER_BOUND('',#3037,.T.);
#1958=FACE_OUTER_BOUND('',#3038,.T.);
#1959=FACE_OUTER_BOUND('',#3039,.T.);
#1960=FACE_OUTER_BOUND('',#3040,.T.);
#1961=FACE_OUTER_BOUND('',#3041,.T.);
#1962=FACE_OUTER_BOUND('',#3042,.T.);
#1963=FACE_OUTER_BOUND('',#3043,.T.);
#1964=FACE_OUTER_BOUND('',#3044,.T.);
#1965=FACE_OUTER_BOUND('',#3045,.T.);
#1966=FACE_OUTER_BOUND('',#3046,.T.);
#1967=FACE_OUTER_BOUND('',#3047,.T.);
#1968=FACE_OUTER_BOUND('',#3048,.T.);
#1969=FACE_OUTER_BOUND('',#3051,.T.);
#1970=FACE_OUTER_BOUND('',#3052,.T.);
#1971=FACE_OUTER_BOUND('',#3053,.T.);
#1972=FACE_OUTER_BOUND('',#3054,.T.);
#1973=FACE_OUTER_BOUND('',#3055,.T.);
#1974=FACE_OUTER_BOUND('',#3056,.T.);
#1975=FACE_OUTER_BOUND('',#3057,.T.);
#1976=FACE_OUTER_BOUND('',#3058,.T.);
#1977=FACE_OUTER_BOUND('',#3059,.T.);
#1978=FACE_OUTER_BOUND('',#3060,.T.);
#1979=FACE_OUTER_BOUND('',#3061,.T.);
#1980=FACE_OUTER_BOUND('',#3062,.T.);
#1981=FACE_OUTER_BOUND('',#3063,.T.);
#1982=FACE_OUTER_BOUND('',#3064,.T.);
#1983=FACE_OUTER_BOUND('',#3065,.T.);
#1984=FACE_OUTER_BOUND('',#3066,.T.);
#1985=FACE_OUTER_BOUND('',#3067,.T.);
#1986=FACE_OUTER_BOUND('',#3068,.T.);
#1987=FACE_OUTER_BOUND('',#3069,.T.);
#1988=FACE_OUTER_BOUND('',#3070,.T.);
#1989=FACE_OUTER_BOUND('',#3071,.T.);
#1990=FACE_OUTER_BOUND('',#3072,.T.);
#1991=FACE_OUTER_BOUND('',#3073,.T.);
#1992=FACE_OUTER_BOUND('',#3074,.T.);
#1993=FACE_OUTER_BOUND('',#3075,.T.);
#1994=FACE_OUTER_BOUND('',#3076,.T.);
#1995=FACE_OUTER_BOUND('',#3077,.T.);
#1996=FACE_OUTER_BOUND('',#3078,.T.);
#1997=FACE_OUTER_BOUND('',#3079,.T.);
#1998=FACE_OUTER_BOUND('',#3080,.T.);
#1999=FACE_OUTER_BOUND('',#3081,.T.);
#2000=FACE_OUTER_BOUND('',#3082,.T.);
#2001=FACE_OUTER_BOUND('',#3083,.T.);
#2002=FACE_OUTER_BOUND('',#3084,.T.);
#2003=FACE_OUTER_BOUND('',#3085,.T.);
#2004=FACE_OUTER_BOUND('',#3086,.T.);
#2005=FACE_OUTER_BOUND('',#3087,.T.);
#2006=FACE_OUTER_BOUND('',#3088,.T.);
#2007=FACE_OUTER_BOUND('',#3089,.T.);
#2008=FACE_OUTER_BOUND('',#3090,.T.);
#2009=FACE_OUTER_BOUND('',#3091,.T.);
#2010=FACE_OUTER_BOUND('',#3092,.T.);
#2011=FACE_OUTER_BOUND('',#3093,.T.);
#2012=FACE_OUTER_BOUND('',#3094,.T.);
#2013=FACE_OUTER_BOUND('',#3095,.T.);
#2014=FACE_OUTER_BOUND('',#3096,.T.);
#2015=FACE_OUTER_BOUND('',#3097,.T.);
#2016=FACE_OUTER_BOUND('',#3098,.T.);
#2017=FACE_OUTER_BOUND('',#3099,.T.);
#2018=FACE_OUTER_BOUND('',#3100,.T.);
#2019=FACE_OUTER_BOUND('',#3101,.T.);
#2020=FACE_OUTER_BOUND('',#3102,.T.);
#2021=FACE_OUTER_BOUND('',#3103,.T.);
#2022=FACE_OUTER_BOUND('',#3104,.T.);
#2023=FACE_OUTER_BOUND('',#3105,.T.);
#2024=FACE_OUTER_BOUND('',#3106,.T.);
#2025=FACE_OUTER_BOUND('',#3107,.T.);
#2026=FACE_OUTER_BOUND('',#3108,.T.);
#2027=FACE_OUTER_BOUND('',#3109,.T.);
#2028=FACE_OUTER_BOUND('',#3110,.T.);
#2029=FACE_OUTER_BOUND('',#3111,.T.);
#2030=FACE_OUTER_BOUND('',#3112,.T.);
#2031=FACE_OUTER_BOUND('',#3113,.T.);
#2032=FACE_OUTER_BOUND('',#3114,.T.);
#2033=FACE_OUTER_BOUND('',#3115,.T.);
#2034=FACE_OUTER_BOUND('',#3116,.T.);
#2035=FACE_OUTER_BOUND('',#3117,.T.);
#2036=FACE_OUTER_BOUND('',#3118,.T.);
#2037=FACE_OUTER_BOUND('',#3119,.T.);
#2038=FACE_OUTER_BOUND('',#3120,.T.);
#2039=FACE_OUTER_BOUND('',#3121,.T.);
#2040=FACE_OUTER_BOUND('',#3122,.T.);
#2041=FACE_OUTER_BOUND('',#3123,.T.);
#2042=FACE_OUTER_BOUND('',#3124,.T.);
#2043=FACE_OUTER_BOUND('',#3125,.T.);
#2044=FACE_OUTER_BOUND('',#3126,.T.);
#2045=FACE_OUTER_BOUND('',#3127,.T.);
#2046=FACE_OUTER_BOUND('',#3128,.T.);
#2047=FACE_OUTER_BOUND('',#3129,.T.);
#2048=FACE_OUTER_BOUND('',#3130,.T.);
#2049=FACE_OUTER_BOUND('',#3131,.T.);
#2050=FACE_OUTER_BOUND('',#3132,.T.);
#2051=FACE_OUTER_BOUND('',#3133,.T.);
#2052=FACE_OUTER_BOUND('',#3134,.T.);
#2053=FACE_OUTER_BOUND('',#3135,.T.);
#2054=FACE_OUTER_BOUND('',#3136,.T.);
#2055=FACE_OUTER_BOUND('',#3137,.T.);
#2056=FACE_OUTER_BOUND('',#3138,.T.);
#2057=FACE_OUTER_BOUND('',#3139,.T.);
#2058=FACE_OUTER_BOUND('',#3140,.T.);
#2059=FACE_OUTER_BOUND('',#3141,.T.);
#2060=FACE_OUTER_BOUND('',#3142,.T.);
#2061=FACE_OUTER_BOUND('',#3143,.T.);
#2062=FACE_OUTER_BOUND('',#3144,.T.);
#2063=FACE_OUTER_BOUND('',#3145,.T.);
#2064=FACE_OUTER_BOUND('',#3146,.T.);
#2065=FACE_OUTER_BOUND('',#3147,.T.);
#2066=FACE_OUTER_BOUND('',#3148,.T.);
#2067=FACE_OUTER_BOUND('',#3149,.T.);
#2068=FACE_OUTER_BOUND('',#3150,.T.);
#2069=FACE_OUTER_BOUND('',#3151,.T.);
#2070=FACE_OUTER_BOUND('',#3152,.T.);
#2071=FACE_OUTER_BOUND('',#3153,.T.);
#2072=FACE_OUTER_BOUND('',#3155,.T.);
#2073=FACE_OUTER_BOUND('',#3156,.T.);
#2074=FACE_OUTER_BOUND('',#3157,.T.);
#2075=FACE_OUTER_BOUND('',#3158,.T.);
#2076=FACE_OUTER_BOUND('',#3159,.T.);
#2077=FACE_OUTER_BOUND('',#3160,.T.);
#2078=FACE_OUTER_BOUND('',#3161,.T.);
#2079=FACE_OUTER_BOUND('',#3162,.T.);
#2080=FACE_OUTER_BOUND('',#3163,.T.);
#2081=FACE_OUTER_BOUND('',#3164,.T.);
#2082=FACE_OUTER_BOUND('',#3165,.T.);
#2083=FACE_OUTER_BOUND('',#3166,.T.);
#2084=FACE_OUTER_BOUND('',#3167,.T.);
#2085=FACE_OUTER_BOUND('',#3169,.T.);
#2086=FACE_OUTER_BOUND('',#3170,.T.);
#2087=FACE_OUTER_BOUND('',#3171,.T.);
#2088=FACE_OUTER_BOUND('',#3172,.T.);
#2089=FACE_OUTER_BOUND('',#3173,.T.);
#2090=FACE_OUTER_BOUND('',#3174,.T.);
#2091=FACE_OUTER_BOUND('',#3175,.T.);
#2092=FACE_OUTER_BOUND('',#3176,.T.);
#2093=FACE_OUTER_BOUND('',#3177,.T.);
#2094=FACE_OUTER_BOUND('',#3179,.T.);
#2095=FACE_OUTER_BOUND('',#3181,.T.);
#2096=FACE_OUTER_BOUND('',#3182,.T.);
#2097=FACE_OUTER_BOUND('',#3184,.T.);
#2098=FACE_OUTER_BOUND('',#3185,.T.);
#2099=FACE_OUTER_BOUND('',#3186,.T.);
#2100=FACE_OUTER_BOUND('',#3187,.T.);
#2101=FACE_OUTER_BOUND('',#3188,.T.);
#2102=FACE_OUTER_BOUND('',#3189,.T.);
#2103=FACE_OUTER_BOUND('',#3190,.T.);
#2104=FACE_OUTER_BOUND('',#3191,.T.);
#2105=FACE_OUTER_BOUND('',#3192,.T.);
#2106=FACE_OUTER_BOUND('',#3193,.T.);
#2107=FACE_OUTER_BOUND('',#3194,.T.);
#2108=FACE_OUTER_BOUND('',#3195,.T.);
#2109=FACE_OUTER_BOUND('',#3196,.T.);
#2110=FACE_OUTER_BOUND('',#3197,.T.);
#2111=FACE_OUTER_BOUND('',#3198,.T.);
#2112=FACE_OUTER_BOUND('',#3199,.T.);
#2113=FACE_OUTER_BOUND('',#3200,.T.);
#2114=FACE_OUTER_BOUND('',#3201,.T.);
#2115=FACE_OUTER_BOUND('',#3202,.T.);
#2116=FACE_OUTER_BOUND('',#3203,.T.);
#2117=FACE_OUTER_BOUND('',#3204,.T.);
#2118=FACE_OUTER_BOUND('',#3205,.T.);
#2119=FACE_OUTER_BOUND('',#3206,.T.);
#2120=FACE_OUTER_BOUND('',#3207,.T.);
#2121=FACE_OUTER_BOUND('',#3208,.T.);
#2122=FACE_OUTER_BOUND('',#3209,.T.);
#2123=FACE_OUTER_BOUND('',#3210,.T.);
#2124=FACE_OUTER_BOUND('',#3211,.T.);
#2125=FACE_OUTER_BOUND('',#3212,.T.);
#2126=FACE_OUTER_BOUND('',#3213,.T.);
#2127=FACE_OUTER_BOUND('',#3214,.T.);
#2128=FACE_OUTER_BOUND('',#3215,.T.);
#2129=FACE_OUTER_BOUND('',#3216,.T.);
#2130=FACE_OUTER_BOUND('',#3217,.T.);
#2131=FACE_OUTER_BOUND('',#3218,.T.);
#2132=FACE_OUTER_BOUND('',#3219,.T.);
#2133=FACE_OUTER_BOUND('',#3220,.T.);
#2134=FACE_OUTER_BOUND('',#3221,.T.);
#2135=FACE_OUTER_BOUND('',#3222,.T.);
#2136=FACE_OUTER_BOUND('',#3223,.T.);
#2137=FACE_OUTER_BOUND('',#3224,.T.);
#2138=FACE_OUTER_BOUND('',#3225,.T.);
#2139=FACE_OUTER_BOUND('',#3226,.T.);
#2140=FACE_OUTER_BOUND('',#3227,.T.);
#2141=FACE_OUTER_BOUND('',#3228,.T.);
#2142=FACE_OUTER_BOUND('',#3229,.T.);
#2143=FACE_OUTER_BOUND('',#3230,.T.);
#2144=FACE_OUTER_BOUND('',#3231,.T.);
#2145=FACE_OUTER_BOUND('',#3232,.T.);
#2146=FACE_OUTER_BOUND('',#3233,.T.);
#2147=FACE_OUTER_BOUND('',#3234,.T.);
#2148=FACE_OUTER_BOUND('',#3235,.T.);
#2149=FACE_OUTER_BOUND('',#3236,.T.);
#2150=FACE_OUTER_BOUND('',#3237,.T.);
#2151=FACE_OUTER_BOUND('',#3238,.T.);
#2152=FACE_OUTER_BOUND('',#3239,.T.);
#2153=FACE_OUTER_BOUND('',#3240,.T.);
#2154=FACE_OUTER_BOUND('',#3241,.T.);
#2155=FACE_OUTER_BOUND('',#3242,.T.);
#2156=FACE_OUTER_BOUND('',#3243,.T.);
#2157=FACE_OUTER_BOUND('',#3244,.T.);
#2158=FACE_OUTER_BOUND('',#3245,.T.);
#2159=FACE_OUTER_BOUND('',#3246,.T.);
#2160=FACE_OUTER_BOUND('',#3247,.T.);
#2161=FACE_OUTER_BOUND('',#3248,.T.);
#2162=FACE_OUTER_BOUND('',#3249,.T.);
#2163=FACE_OUTER_BOUND('',#3250,.T.);
#2164=FACE_OUTER_BOUND('',#3251,.T.);
#2165=FACE_OUTER_BOUND('',#3252,.T.);
#2166=FACE_OUTER_BOUND('',#3253,.T.);
#2167=FACE_OUTER_BOUND('',#3254,.T.);
#2168=FACE_OUTER_BOUND('',#3255,.T.);
#2169=FACE_OUTER_BOUND('',#3256,.T.);
#2170=FACE_OUTER_BOUND('',#3257,.T.);
#2171=FACE_OUTER_BOUND('',#3258,.T.);
#2172=FACE_OUTER_BOUND('',#3259,.T.);
#2173=FACE_OUTER_BOUND('',#3260,.T.);
#2174=FACE_OUTER_BOUND('',#3261,.T.);
#2175=FACE_OUTER_BOUND('',#3262,.T.);
#2176=FACE_OUTER_BOUND('',#3263,.T.);
#2177=FACE_OUTER_BOUND('',#3264,.T.);
#2178=FACE_OUTER_BOUND('',#3265,.T.);
#2179=FACE_OUTER_BOUND('',#3266,.T.);
#2180=FACE_OUTER_BOUND('',#3267,.T.);
#2181=FACE_OUTER_BOUND('',#3268,.T.);
#2182=FACE_OUTER_BOUND('',#3269,.T.);
#2183=FACE_OUTER_BOUND('',#3270,.T.);
#2184=FACE_OUTER_BOUND('',#3271,.T.);
#2185=FACE_OUTER_BOUND('',#3272,.T.);
#2186=FACE_OUTER_BOUND('',#3273,.T.);
#2187=FACE_OUTER_BOUND('',#3274,.T.);
#2188=FACE_OUTER_BOUND('',#3275,.T.);
#2189=FACE_OUTER_BOUND('',#3276,.T.);
#2190=FACE_OUTER_BOUND('',#3277,.T.);
#2191=FACE_OUTER_BOUND('',#3278,.T.);
#2192=FACE_OUTER_BOUND('',#3279,.T.);
#2193=FACE_OUTER_BOUND('',#3280,.T.);
#2194=FACE_OUTER_BOUND('',#3281,.T.);
#2195=FACE_OUTER_BOUND('',#3282,.T.);
#2196=FACE_OUTER_BOUND('',#3283,.T.);
#2197=FACE_OUTER_BOUND('',#3289,.T.);
#2198=FACE_OUTER_BOUND('',#3291,.T.);
#2199=FACE_OUTER_BOUND('',#3292,.T.);
#2200=FACE_OUTER_BOUND('',#3294,.T.);
#2201=FACE_OUTER_BOUND('',#3296,.T.);
#2202=FACE_OUTER_BOUND('',#3297,.T.);
#2203=FACE_OUTER_BOUND('',#3298,.T.);
#2204=FACE_OUTER_BOUND('',#3299,.T.);
#2205=FACE_OUTER_BOUND('',#3300,.T.);
#2206=FACE_OUTER_BOUND('',#3301,.T.);
#2207=FACE_OUTER_BOUND('',#3302,.T.);
#2208=FACE_OUTER_BOUND('',#3303,.T.);
#2209=FACE_OUTER_BOUND('',#3304,.T.);
#2210=FACE_OUTER_BOUND('',#3305,.T.);
#2211=FACE_OUTER_BOUND('',#3306,.T.);
#2212=FACE_OUTER_BOUND('',#3307,.T.);
#2213=FACE_OUTER_BOUND('',#3308,.T.);
#2214=FACE_OUTER_BOUND('',#3309,.T.);
#2215=FACE_OUTER_BOUND('',#3311,.T.);
#2216=FACE_OUTER_BOUND('',#3313,.T.);
#2217=FACE_OUTER_BOUND('',#3314,.T.);
#2218=FACE_OUTER_BOUND('',#3315,.T.);
#2219=FACE_OUTER_BOUND('',#3316,.T.);
#2220=FACE_OUTER_BOUND('',#3317,.T.);
#2221=FACE_OUTER_BOUND('',#3318,.T.);
#2222=FACE_OUTER_BOUND('',#3319,.T.);
#2223=FACE_OUTER_BOUND('',#3320,.T.);
#2224=FACE_OUTER_BOUND('',#3321,.T.);
#2225=FACE_OUTER_BOUND('',#3322,.T.);
#2226=FACE_OUTER_BOUND('',#3323,.T.);
#2227=FACE_OUTER_BOUND('',#3324,.T.);
#2228=FACE_OUTER_BOUND('',#3325,.T.);
#2229=FACE_OUTER_BOUND('',#3326,.T.);
#2230=FACE_OUTER_BOUND('',#3327,.T.);
#2231=FACE_OUTER_BOUND('',#3328,.T.);
#2232=FACE_OUTER_BOUND('',#3329,.T.);
#2233=FACE_OUTER_BOUND('',#3330,.T.);
#2234=FACE_OUTER_BOUND('',#3331,.T.);
#2235=FACE_OUTER_BOUND('',#3332,.T.);
#2236=FACE_OUTER_BOUND('',#3333,.T.);
#2237=FACE_OUTER_BOUND('',#3334,.T.);
#2238=FACE_OUTER_BOUND('',#3335,.T.);
#2239=FACE_OUTER_BOUND('',#3336,.T.);
#2240=FACE_OUTER_BOUND('',#3337,.T.);
#2241=FACE_OUTER_BOUND('',#3338,.T.);
#2242=FACE_OUTER_BOUND('',#3339,.T.);
#2243=FACE_OUTER_BOUND('',#3340,.T.);
#2244=FACE_OUTER_BOUND('',#3341,.T.);
#2245=FACE_OUTER_BOUND('',#3342,.T.);
#2246=FACE_OUTER_BOUND('',#3343,.T.);
#2247=FACE_OUTER_BOUND('',#3344,.T.);
#2248=FACE_OUTER_BOUND('',#3345,.T.);
#2249=FACE_OUTER_BOUND('',#3346,.T.);
#2250=FACE_OUTER_BOUND('',#3347,.T.);
#2251=FACE_OUTER_BOUND('',#3348,.T.);
#2252=FACE_OUTER_BOUND('',#3349,.T.);
#2253=FACE_OUTER_BOUND('',#3350,.T.);
#2254=FACE_OUTER_BOUND('',#3351,.T.);
#2255=FACE_OUTER_BOUND('',#3352,.T.);
#2256=FACE_OUTER_BOUND('',#3353,.T.);
#2257=FACE_OUTER_BOUND('',#3356,.T.);
#2258=FACE_OUTER_BOUND('',#3357,.T.);
#2259=FACE_OUTER_BOUND('',#3360,.T.);
#2260=FACE_OUTER_BOUND('',#3363,.T.);
#2261=FACE_OUTER_BOUND('',#3364,.T.);
#2262=FACE_OUTER_BOUND('',#3365,.T.);
#2263=FACE_OUTER_BOUND('',#3366,.T.);
#2264=FACE_OUTER_BOUND('',#3368,.T.);
#2265=FACE_OUTER_BOUND('',#3369,.T.);
#2266=FACE_OUTER_BOUND('',#3370,.T.);
#2267=FACE_OUTER_BOUND('',#3372,.T.);
#2268=FACE_OUTER_BOUND('',#3374,.T.);
#2269=FACE_OUTER_BOUND('',#3375,.T.);
#2270=FACE_OUTER_BOUND('',#3376,.T.);
#2271=FACE_OUTER_BOUND('',#3377,.T.);
#2272=FACE_OUTER_BOUND('',#3378,.T.);
#2273=FACE_OUTER_BOUND('',#3379,.T.);
#2274=FACE_OUTER_BOUND('',#3380,.T.);
#2275=FACE_OUTER_BOUND('',#3383,.T.);
#2276=FACE_OUTER_BOUND('',#3384,.T.);
#2277=FACE_OUTER_BOUND('',#3385,.T.);
#2278=FACE_OUTER_BOUND('',#3386,.T.);
#2279=FACE_OUTER_BOUND('',#3388,.T.);
#2280=FACE_OUTER_BOUND('',#3389,.T.);
#2281=FACE_OUTER_BOUND('',#3390,.T.);
#2282=FACE_OUTER_BOUND('',#3391,.T.);
#2283=FACE_OUTER_BOUND('',#3392,.T.);
#2284=FACE_OUTER_BOUND('',#3393,.T.);
#2285=FACE_OUTER_BOUND('',#3394,.T.);
#2286=FACE_OUTER_BOUND('',#3395,.T.);
#2287=FACE_OUTER_BOUND('',#3398,.T.);
#2288=FACE_OUTER_BOUND('',#3400,.T.);
#2289=FACE_OUTER_BOUND('',#3401,.T.);
#2290=FACE_OUTER_BOUND('',#3402,.T.);
#2291=FACE_OUTER_BOUND('',#3403,.T.);
#2292=FACE_OUTER_BOUND('',#3404,.T.);
#2293=FACE_OUTER_BOUND('',#3405,.T.);
#2294=FACE_OUTER_BOUND('',#3406,.T.);
#2295=FACE_OUTER_BOUND('',#3407,.T.);
#2296=FACE_OUTER_BOUND('',#3408,.T.);
#2297=FACE_OUTER_BOUND('',#3409,.T.);
#2298=FACE_OUTER_BOUND('',#3410,.T.);
#2299=FACE_OUTER_BOUND('',#3411,.T.);
#2300=FACE_OUTER_BOUND('',#3412,.T.);
#2301=FACE_OUTER_BOUND('',#3413,.T.);
#2302=FACE_OUTER_BOUND('',#3414,.T.);
#2303=FACE_OUTER_BOUND('',#3415,.T.);
#2304=FACE_OUTER_BOUND('',#3416,.T.);
#2305=FACE_OUTER_BOUND('',#3417,.T.);
#2306=FACE_OUTER_BOUND('',#3418,.T.);
#2307=FACE_OUTER_BOUND('',#3419,.T.);
#2308=FACE_OUTER_BOUND('',#3420,.T.);
#2309=FACE_OUTER_BOUND('',#3421,.T.);
#2310=FACE_OUTER_BOUND('',#3422,.T.);
#2311=FACE_OUTER_BOUND('',#3423,.T.);
#2312=FACE_OUTER_BOUND('',#3424,.T.);
#2313=FACE_OUTER_BOUND('',#3425,.T.);
#2314=FACE_OUTER_BOUND('',#3426,.T.);
#2315=FACE_OUTER_BOUND('',#3427,.T.);
#2316=FACE_OUTER_BOUND('',#3428,.T.);
#2317=FACE_OUTER_BOUND('',#3429,.T.);
#2318=FACE_OUTER_BOUND('',#3430,.T.);
#2319=FACE_OUTER_BOUND('',#3431,.T.);
#2320=FACE_OUTER_BOUND('',#3432,.T.);
#2321=FACE_OUTER_BOUND('',#3433,.T.);
#2322=FACE_OUTER_BOUND('',#3434,.T.);
#2323=FACE_OUTER_BOUND('',#3435,.T.);
#2324=FACE_OUTER_BOUND('',#3436,.T.);
#2325=FACE_OUTER_BOUND('',#3437,.T.);
#2326=FACE_OUTER_BOUND('',#3438,.T.);
#2327=FACE_OUTER_BOUND('',#3439,.T.);
#2328=FACE_OUTER_BOUND('',#3441,.T.);
#2329=FACE_OUTER_BOUND('',#3443,.T.);
#2330=FACE_OUTER_BOUND('',#3445,.T.);
#2331=FACE_OUTER_BOUND('',#3446,.T.);
#2332=FACE_OUTER_BOUND('',#3447,.T.);
#2333=FACE_OUTER_BOUND('',#3448,.T.);
#2334=FACE_OUTER_BOUND('',#3449,.T.);
#2335=FACE_OUTER_BOUND('',#3450,.T.);
#2336=FACE_OUTER_BOUND('',#3451,.T.);
#2337=FACE_OUTER_BOUND('',#3452,.T.);
#2338=FACE_OUTER_BOUND('',#3453,.T.);
#2339=FACE_OUTER_BOUND('',#3454,.T.);
#2340=FACE_OUTER_BOUND('',#3455,.T.);
#2341=FACE_OUTER_BOUND('',#3457,.T.);
#2342=FACE_OUTER_BOUND('',#3458,.T.);
#2343=FACE_OUTER_BOUND('',#3459,.T.);
#2344=FACE_OUTER_BOUND('',#3460,.T.);
#2345=FACE_OUTER_BOUND('',#3461,.T.);
#2346=FACE_OUTER_BOUND('',#3462,.T.);
#2347=FACE_OUTER_BOUND('',#3463,.T.);
#2348=FACE_OUTER_BOUND('',#3464,.T.);
#2349=FACE_OUTER_BOUND('',#3465,.T.);
#2350=FACE_OUTER_BOUND('',#3468,.T.);
#2351=FACE_OUTER_BOUND('',#3469,.T.);
#2352=FACE_OUTER_BOUND('',#3472,.T.);
#2353=FACE_OUTER_BOUND('',#3473,.T.);
#2354=FACE_OUTER_BOUND('',#3474,.T.);
#2355=FACE_OUTER_BOUND('',#3475,.T.);
#2356=FACE_OUTER_BOUND('',#3476,.T.);
#2357=FACE_OUTER_BOUND('',#3477,.T.);
#2358=FACE_OUTER_BOUND('',#3478,.T.);
#2359=FACE_OUTER_BOUND('',#3479,.T.);
#2360=FACE_OUTER_BOUND('',#3480,.T.);
#2361=FACE_OUTER_BOUND('',#3481,.T.);
#2362=FACE_OUTER_BOUND('',#3482,.T.);
#2363=FACE_OUTER_BOUND('',#3483,.T.);
#2364=FACE_OUTER_BOUND('',#3484,.T.);
#2365=FACE_OUTER_BOUND('',#3485,.T.);
#2366=FACE_OUTER_BOUND('',#3486,.T.);
#2367=FACE_OUTER_BOUND('',#3487,.T.);
#2368=FACE_OUTER_BOUND('',#3489,.T.);
#2369=FACE_OUTER_BOUND('',#3490,.T.);
#2370=FACE_OUTER_BOUND('',#3491,.T.);
#2371=FACE_OUTER_BOUND('',#3492,.T.);
#2372=FACE_OUTER_BOUND('',#3493,.T.);
#2373=FACE_OUTER_BOUND('',#3494,.T.);
#2374=FACE_OUTER_BOUND('',#3495,.T.);
#2375=FACE_OUTER_BOUND('',#3496,.T.);
#2376=FACE_OUTER_BOUND('',#3498,.T.);
#2377=FACE_OUTER_BOUND('',#3499,.T.);
#2378=FACE_OUTER_BOUND('',#3500,.T.);
#2379=FACE_OUTER_BOUND('',#3501,.T.);
#2380=FACE_OUTER_BOUND('',#3502,.T.);
#2381=FACE_OUTER_BOUND('',#3504,.T.);
#2382=FACE_OUTER_BOUND('',#3505,.T.);
#2383=FACE_OUTER_BOUND('',#3506,.T.);
#2384=FACE_OUTER_BOUND('',#3507,.T.);
#2385=FACE_OUTER_BOUND('',#3508,.T.);
#2386=FACE_OUTER_BOUND('',#3509,.T.);
#2387=FACE_OUTER_BOUND('',#3510,.T.);
#2388=FACE_OUTER_BOUND('',#3511,.T.);
#2389=FACE_OUTER_BOUND('',#3512,.T.);
#2390=FACE_OUTER_BOUND('',#3513,.T.);
#2391=FACE_OUTER_BOUND('',#3514,.T.);
#2392=FACE_OUTER_BOUND('',#3515,.T.);
#2393=FACE_OUTER_BOUND('',#3516,.T.);
#2394=FACE_OUTER_BOUND('',#3517,.T.);
#2395=FACE_OUTER_BOUND('',#3518,.T.);
#2396=FACE_OUTER_BOUND('',#3519,.T.);
#2397=FACE_OUTER_BOUND('',#3521,.T.);
#2398=FACE_OUTER_BOUND('',#3522,.T.);
#2399=FACE_OUTER_BOUND('',#3523,.T.);
#2400=FACE_OUTER_BOUND('',#3524,.T.);
#2401=FACE_OUTER_BOUND('',#3525,.T.);
#2402=FACE_OUTER_BOUND('',#3526,.T.);
#2403=FACE_OUTER_BOUND('',#3527,.T.);
#2404=FACE_OUTER_BOUND('',#3528,.T.);
#2405=FACE_OUTER_BOUND('',#3529,.T.);
#2406=FACE_OUTER_BOUND('',#3530,.T.);
#2407=FACE_OUTER_BOUND('',#3531,.T.);
#2408=FACE_OUTER_BOUND('',#3532,.T.);
#2409=FACE_OUTER_BOUND('',#3533,.T.);
#2410=FACE_OUTER_BOUND('',#3534,.T.);
#2411=FACE_OUTER_BOUND('',#3535,.T.);
#2412=FACE_OUTER_BOUND('',#3536,.T.);
#2413=FACE_OUTER_BOUND('',#3537,.T.);
#2414=FACE_OUTER_BOUND('',#3538,.T.);
#2415=FACE_OUTER_BOUND('',#3539,.T.);
#2416=FACE_OUTER_BOUND('',#3540,.T.);
#2417=FACE_OUTER_BOUND('',#3541,.T.);
#2418=FACE_OUTER_BOUND('',#3542,.T.);
#2419=FACE_OUTER_BOUND('',#3543,.T.);
#2420=FACE_OUTER_BOUND('',#3544,.T.);
#2421=FACE_OUTER_BOUND('',#3545,.T.);
#2422=FACE_OUTER_BOUND('',#3546,.T.);
#2423=FACE_OUTER_BOUND('',#3547,.T.);
#2424=FACE_OUTER_BOUND('',#3548,.T.);
#2425=FACE_OUTER_BOUND('',#3549,.T.);
#2426=FACE_OUTER_BOUND('',#3550,.T.);
#2427=FACE_OUTER_BOUND('',#3551,.T.);
#2428=FACE_OUTER_BOUND('',#3552,.T.);
#2429=FACE_OUTER_BOUND('',#3553,.T.);
#2430=FACE_OUTER_BOUND('',#3554,.T.);
#2431=FACE_OUTER_BOUND('',#3555,.T.);
#2432=FACE_OUTER_BOUND('',#3556,.T.);
#2433=FACE_OUTER_BOUND('',#3557,.T.);
#2434=FACE_OUTER_BOUND('',#3558,.T.);
#2435=FACE_OUTER_BOUND('',#3559,.T.);
#2436=FACE_OUTER_BOUND('',#3560,.T.);
#2437=FACE_OUTER_BOUND('',#3561,.T.);
#2438=FACE_OUTER_BOUND('',#3562,.T.);
#2439=FACE_OUTER_BOUND('',#3563,.T.);
#2440=FACE_OUTER_BOUND('',#3564,.T.);
#2441=FACE_OUTER_BOUND('',#3565,.T.);
#2442=FACE_OUTER_BOUND('',#3567,.T.);
#2443=FACE_OUTER_BOUND('',#3569,.T.);
#2444=FACE_OUTER_BOUND('',#3570,.T.);
#2445=FACE_OUTER_BOUND('',#3571,.T.);
#2446=FACE_OUTER_BOUND('',#3572,.T.);
#2447=FACE_OUTER_BOUND('',#3573,.T.);
#2448=FACE_OUTER_BOUND('',#3574,.T.);
#2449=FACE_OUTER_BOUND('',#3575,.T.);
#2450=FACE_OUTER_BOUND('',#3576,.T.);
#2451=FACE_OUTER_BOUND('',#3577,.T.);
#2452=FACE_OUTER_BOUND('',#3578,.T.);
#2453=FACE_OUTER_BOUND('',#3579,.T.);
#2454=FACE_OUTER_BOUND('',#3580,.T.);
#2455=FACE_OUTER_BOUND('',#3581,.T.);
#2456=FACE_OUTER_BOUND('',#3582,.T.);
#2457=FACE_OUTER_BOUND('',#3584,.T.);
#2458=EDGE_LOOP('',(#11214,#11215,#11216,#11217));
#2459=EDGE_LOOP('',(#11218));
#2460=EDGE_LOOP('',(#11219));
#2461=EDGE_LOOP('',(#11220));
#2462=EDGE_LOOP('',(#11221));
#2463=EDGE_LOOP('',(#11222));
#2464=EDGE_LOOP('',(#11223));
#2465=EDGE_LOOP('',(#11224));
#2466=EDGE_LOOP('',(#11225));
#2467=EDGE_LOOP('',(#11226));
#2468=EDGE_LOOP('',(#11227));
#2469=EDGE_LOOP('',(#11228));
#2470=EDGE_LOOP('',(#11229));
#2471=EDGE_LOOP('',(#11230));
#2472=EDGE_LOOP('',(#11231));
#2473=EDGE_LOOP('',(#11232));
#2474=EDGE_LOOP('',(#11233));
#2475=EDGE_LOOP('',(#11234));
#2476=EDGE_LOOP('',(#11235));
#2477=EDGE_LOOP('',(#11236));
#2478=EDGE_LOOP('',(#11237));
#2479=EDGE_LOOP('',(#11238));
#2480=EDGE_LOOP('',(#11239));
#2481=EDGE_LOOP('',(#11240));
#2482=EDGE_LOOP('',(#11241));
#2483=EDGE_LOOP('',(#11242));
#2484=EDGE_LOOP('',(#11243));
#2485=EDGE_LOOP('',(#11244,#11245,#11246,#11247));
#2486=EDGE_LOOP('',(#11248,#11249,#11250,#11251));
#2487=EDGE_LOOP('',(#11252,#11253,#11254,#11255));
#2488=EDGE_LOOP('',(#11256,#11257,#11258,#11259));
#2489=EDGE_LOOP('',(#11260,#11261,#11262,#11263));
#2490=EDGE_LOOP('',(#11264,#11265,#11266,#11267));
#2491=EDGE_LOOP('',(#11268,#11269,#11270,#11271));
#2492=EDGE_LOOP('',(#11272,#11273,#11274,#11275));
#2493=EDGE_LOOP('',(#11276,#11277,#11278,#11279));
#2494=EDGE_LOOP('',(#11280,#11281,#11282,#11283));
#2495=EDGE_LOOP('',(#11284,#11285,#11286,#11287));
#2496=EDGE_LOOP('',(#11288,#11289,#11290,#11291));
#2497=EDGE_LOOP('',(#11292,#11293,#11294,#11295));
#2498=EDGE_LOOP('',(#11296,#11297,#11298,#11299));
#2499=EDGE_LOOP('',(#11300,#11301,#11302,#11303));
#2500=EDGE_LOOP('',(#11304,#11305,#11306,#11307));
#2501=EDGE_LOOP('',(#11308,#11309,#11310,#11311));
#2502=EDGE_LOOP('',(#11312,#11313,#11314,#11315));
#2503=EDGE_LOOP('',(#11316,#11317,#11318,#11319));
#2504=EDGE_LOOP('',(#11320,#11321,#11322,#11323));
#2505=EDGE_LOOP('',(#11324,#11325,#11326,#11327));
#2506=EDGE_LOOP('',(#11328,#11329,#11330,#11331));
#2507=EDGE_LOOP('',(#11332,#11333,#11334,#11335));
#2508=EDGE_LOOP('',(#11336,#11337,#11338,#11339));
#2509=EDGE_LOOP('',(#11340,#11341,#11342,#11343));
#2510=EDGE_LOOP('',(#11344,#11345,#11346,#11347));
#2511=EDGE_LOOP('',(#11348,#11349,#11350,#11351));
#2512=EDGE_LOOP('',(#11352,#11353,#11354,#11355));
#2513=EDGE_LOOP('',(#11356,#11357,#11358,#11359));
#2514=EDGE_LOOP('',(#11360,#11361,#11362,#11363));
#2515=EDGE_LOOP('',(#11364,#11365,#11366,#11367));
#2516=EDGE_LOOP('',(#11368,#11369,#11370,#11371));
#2517=EDGE_LOOP('',(#11372,#11373,#11374,#11375));
#2518=EDGE_LOOP('',(#11376,#11377,#11378,#11379));
#2519=EDGE_LOOP('',(#11380,#11381,#11382,#11383));
#2520=EDGE_LOOP('',(#11384,#11385,#11386,#11387));
#2521=EDGE_LOOP('',(#11388,#11389,#11390,#11391));
#2522=EDGE_LOOP('',(#11392,#11393,#11394,#11395));
#2523=EDGE_LOOP('',(#11396,#11397,#11398,#11399));
#2524=EDGE_LOOP('',(#11400,#11401,#11402,#11403));
#2525=EDGE_LOOP('',(#11404,#11405,#11406,#11407));
#2526=EDGE_LOOP('',(#11408,#11409,#11410,#11411));
#2527=EDGE_LOOP('',(#11412,#11413,#11414,#11415));
#2528=EDGE_LOOP('',(#11416,#11417,#11418,#11419));
#2529=EDGE_LOOP('',(#11420,#11421,#11422,#11423));
#2530=EDGE_LOOP('',(#11424,#11425,#11426,#11427));
#2531=EDGE_LOOP('',(#11428,#11429,#11430,#11431));
#2532=EDGE_LOOP('',(#11432,#11433,#11434,#11435));
#2533=EDGE_LOOP('',(#11436,#11437,#11438,#11439));
#2534=EDGE_LOOP('',(#11440,#11441,#11442,#11443));
#2535=EDGE_LOOP('',(#11444,#11445,#11446,#11447));
#2536=EDGE_LOOP('',(#11448,#11449,#11450,#11451));
#2537=EDGE_LOOP('',(#11452,#11453,#11454,#11455));
#2538=EDGE_LOOP('',(#11456));
#2539=EDGE_LOOP('',(#11457));
#2540=EDGE_LOOP('',(#11458));
#2541=EDGE_LOOP('',(#11459));
#2542=EDGE_LOOP('',(#11460));
#2543=EDGE_LOOP('',(#11461));
#2544=EDGE_LOOP('',(#11462));
#2545=EDGE_LOOP('',(#11463));
#2546=EDGE_LOOP('',(#11464));
#2547=EDGE_LOOP('',(#11465));
#2548=EDGE_LOOP('',(#11466));
#2549=EDGE_LOOP('',(#11467));
#2550=EDGE_LOOP('',(#11468));
#2551=EDGE_LOOP('',(#11469));
#2552=EDGE_LOOP('',(#11470));
#2553=EDGE_LOOP('',(#11471));
#2554=EDGE_LOOP('',(#11472));
#2555=EDGE_LOOP('',(#11473));
#2556=EDGE_LOOP('',(#11474));
#2557=EDGE_LOOP('',(#11475));
#2558=EDGE_LOOP('',(#11476));
#2559=EDGE_LOOP('',(#11477));
#2560=EDGE_LOOP('',(#11478));
#2561=EDGE_LOOP('',(#11479));
#2562=EDGE_LOOP('',(#11480));
#2563=EDGE_LOOP('',(#11481));
#2564=EDGE_LOOP('',(#11482,#11483,#11484,#11485));
#2565=EDGE_LOOP('',(#11486,#11487,#11488,#11489));
#2566=EDGE_LOOP('',(#11490,#11491,#11492,#11493));
#2567=EDGE_LOOP('',(#11494,#11495,#11496,#11497));
#2568=EDGE_LOOP('',(#11498,#11499,#11500,#11501));
#2569=EDGE_LOOP('',(#11502,#11503,#11504,#11505));
#2570=EDGE_LOOP('',(#11506,#11507,#11508,#11509));
#2571=EDGE_LOOP('',(#11510,#11511,#11512,#11513));
#2572=EDGE_LOOP('',(#11514,#11515,#11516,#11517));
#2573=EDGE_LOOP('',(#11518,#11519,#11520,#11521));
#2574=EDGE_LOOP('',(#11522,#11523,#11524,#11525));
#2575=EDGE_LOOP('',(#11526,#11527,#11528,#11529));
#2576=EDGE_LOOP('',(#11530,#11531,#11532,#11533));
#2577=EDGE_LOOP('',(#11534,#11535,#11536,#11537));
#2578=EDGE_LOOP('',(#11538,#11539,#11540,#11541));
#2579=EDGE_LOOP('',(#11542,#11543,#11544,#11545));
#2580=EDGE_LOOP('',(#11546,#11547,#11548,#11549));
#2581=EDGE_LOOP('',(#11550,#11551,#11552,#11553));
#2582=EDGE_LOOP('',(#11554,#11555,#11556,#11557));
#2583=EDGE_LOOP('',(#11558,#11559,#11560,#11561));
#2584=EDGE_LOOP('',(#11562,#11563,#11564,#11565));
#2585=EDGE_LOOP('',(#11566,#11567,#11568,#11569));
#2586=EDGE_LOOP('',(#11570,#11571,#11572,#11573));
#2587=EDGE_LOOP('',(#11574,#11575,#11576,#11577));
#2588=EDGE_LOOP('',(#11578,#11579,#11580,#11581));
#2589=EDGE_LOOP('',(#11582,#11583,#11584,#11585));
#2590=EDGE_LOOP('',(#11586,#11587,#11588,#11589));
#2591=EDGE_LOOP('',(#11590,#11591,#11592,#11593));
#2592=EDGE_LOOP('',(#11594,#11595,#11596,#11597));
#2593=EDGE_LOOP('',(#11598,#11599,#11600,#11601));
#2594=EDGE_LOOP('',(#11602,#11603,#11604,#11605));
#2595=EDGE_LOOP('',(#11606,#11607,#11608,#11609));
#2596=EDGE_LOOP('',(#11610,#11611,#11612,#11613));
#2597=EDGE_LOOP('',(#11614,#11615,#11616,#11617));
#2598=EDGE_LOOP('',(#11618,#11619,#11620,#11621));
#2599=EDGE_LOOP('',(#11622,#11623,#11624,#11625));
#2600=EDGE_LOOP('',(#11626,#11627,#11628,#11629));
#2601=EDGE_LOOP('',(#11630,#11631,#11632,#11633));
#2602=EDGE_LOOP('',(#11634,#11635,#11636,#11637));
#2603=EDGE_LOOP('',(#11638,#11639,#11640,#11641));
#2604=EDGE_LOOP('',(#11642,#11643,#11644,#11645));
#2605=EDGE_LOOP('',(#11646,#11647,#11648,#11649));
#2606=EDGE_LOOP('',(#11650,#11651,#11652,#11653));
#2607=EDGE_LOOP('',(#11654,#11655,#11656,#11657));
#2608=EDGE_LOOP('',(#11658,#11659,#11660,#11661));
#2609=EDGE_LOOP('',(#11662,#11663,#11664,#11665));
#2610=EDGE_LOOP('',(#11666,#11667,#11668,#11669));
#2611=EDGE_LOOP('',(#11670,#11671,#11672,#11673));
#2612=EDGE_LOOP('',(#11674,#11675,#11676,#11677));
#2613=EDGE_LOOP('',(#11678,#11679,#11680,#11681));
#2614=EDGE_LOOP('',(#11682,#11683,#11684,#11685));
#2615=EDGE_LOOP('',(#11686,#11687,#11688,#11689));
#2616=EDGE_LOOP('',(#11690,#11691,#11692,#11693));
#2617=EDGE_LOOP('',(#11694,#11695,#11696,#11697));
#2618=EDGE_LOOP('',(#11698,#11699,#11700,#11701));
#2619=EDGE_LOOP('',(#11702,#11703,#11704,#11705));
#2620=EDGE_LOOP('',(#11706,#11707,#11708,#11709));
#2621=EDGE_LOOP('',(#11710,#11711,#11712,#11713));
#2622=EDGE_LOOP('',(#11714,#11715,#11716,#11717));
#2623=EDGE_LOOP('',(#11718,#11719,#11720,#11721));
#2624=EDGE_LOOP('',(#11722,#11723,#11724,#11725));
#2625=EDGE_LOOP('',(#11726,#11727,#11728,#11729));
#2626=EDGE_LOOP('',(#11730,#11731,#11732,#11733));
#2627=EDGE_LOOP('',(#11734,#11735,#11736,#11737));
#2628=EDGE_LOOP('',(#11738,#11739,#11740,#11741));
#2629=EDGE_LOOP('',(#11742,#11743,#11744,#11745));
#2630=EDGE_LOOP('',(#11746,#11747,#11748,#11749));
#2631=EDGE_LOOP('',(#11750,#11751,#11752,#11753));
#2632=EDGE_LOOP('',(#11754,#11755,#11756,#11757));
#2633=EDGE_LOOP('',(#11758,#11759,#11760,#11761));
#2634=EDGE_LOOP('',(#11762,#11763,#11764,#11765));
#2635=EDGE_LOOP('',(#11766,#11767,#11768,#11769));
#2636=EDGE_LOOP('',(#11770,#11771,#11772,#11773));
#2637=EDGE_LOOP('',(#11774,#11775,#11776,#11777));
#2638=EDGE_LOOP('',(#11778,#11779,#11780,#11781));
#2639=EDGE_LOOP('',(#11782,#11783,#11784,#11785));
#2640=EDGE_LOOP('',(#11786,#11787,#11788,#11789));
#2641=EDGE_LOOP('',(#11790,#11791,#11792,#11793));
#2642=EDGE_LOOP('',(#11794,#11795,#11796,#11797));
#2643=EDGE_LOOP('',(#11798,#11799,#11800,#11801));
#2644=EDGE_LOOP('',(#11802,#11803,#11804,#11805));
#2645=EDGE_LOOP('',(#11806,#11807,#11808,#11809));
#2646=EDGE_LOOP('',(#11810,#11811,#11812,#11813));
#2647=EDGE_LOOP('',(#11814,#11815,#11816,#11817));
#2648=EDGE_LOOP('',(#11818,#11819,#11820,#11821));
#2649=EDGE_LOOP('',(#11822,#11823,#11824,#11825));
#2650=EDGE_LOOP('',(#11826,#11827,#11828,#11829));
#2651=EDGE_LOOP('',(#11830,#11831,#11832,#11833));
#2652=EDGE_LOOP('',(#11834,#11835,#11836,#11837));
#2653=EDGE_LOOP('',(#11838,#11839,#11840,#11841));
#2654=EDGE_LOOP('',(#11842,#11843,#11844,#11845));
#2655=EDGE_LOOP('',(#11846,#11847,#11848,#11849));
#2656=EDGE_LOOP('',(#11850,#11851,#11852,#11853));
#2657=EDGE_LOOP('',(#11854,#11855,#11856,#11857));
#2658=EDGE_LOOP('',(#11858,#11859,#11860,#11861));
#2659=EDGE_LOOP('',(#11862,#11863,#11864,#11865));
#2660=EDGE_LOOP('',(#11866,#11867,#11868,#11869));
#2661=EDGE_LOOP('',(#11870,#11871,#11872,#11873));
#2662=EDGE_LOOP('',(#11874,#11875,#11876,#11877));
#2663=EDGE_LOOP('',(#11878,#11879,#11880,#11881));
#2664=EDGE_LOOP('',(#11882,#11883,#11884,#11885));
#2665=EDGE_LOOP('',(#11886,#11887,#11888,#11889));
#2666=EDGE_LOOP('',(#11890,#11891,#11892,#11893));
#2667=EDGE_LOOP('',(#11894,#11895,#11896,#11897));
#2668=EDGE_LOOP('',(#11898,#11899,#11900,#11901));
#2669=EDGE_LOOP('',(#11902,#11903,#11904,#11905));
#2670=EDGE_LOOP('',(#11906,#11907,#11908,#11909));
#2671=EDGE_LOOP('',(#11910,#11911,#11912,#11913));
#2672=EDGE_LOOP('',(#11914,#11915,#11916,#11917));
#2673=EDGE_LOOP('',(#11918,#11919,#11920,#11921));
#2674=EDGE_LOOP('',(#11922,#11923,#11924,#11925));
#2675=EDGE_LOOP('',(#11926,#11927,#11928,#11929));
#2676=EDGE_LOOP('',(#11930,#11931,#11932,#11933));
#2677=EDGE_LOOP('',(#11934,#11935,#11936,#11937));
#2678=EDGE_LOOP('',(#11938,#11939,#11940,#11941));
#2679=EDGE_LOOP('',(#11942,#11943,#11944,#11945));
#2680=EDGE_LOOP('',(#11946,#11947,#11948,#11949));
#2681=EDGE_LOOP('',(#11950,#11951,#11952,#11953));
#2682=EDGE_LOOP('',(#11954,#11955,#11956,#11957));
#2683=EDGE_LOOP('',(#11958,#11959,#11960,#11961));
#2684=EDGE_LOOP('',(#11962,#11963,#11964,#11965));
#2685=EDGE_LOOP('',(#11966,#11967,#11968,#11969));
#2686=EDGE_LOOP('',(#11970,#11971,#11972,#11973));
#2687=EDGE_LOOP('',(#11974,#11975,#11976,#11977));
#2688=EDGE_LOOP('',(#11978,#11979,#11980,#11981));
#2689=EDGE_LOOP('',(#11982,#11983,#11984,#11985));
#2690=EDGE_LOOP('',(#11986,#11987,#11988,#11989));
#2691=EDGE_LOOP('',(#11990,#11991,#11992,#11993));
#2692=EDGE_LOOP('',(#11994,#11995,#11996,#11997));
#2693=EDGE_LOOP('',(#11998,#11999,#12000,#12001));
#2694=EDGE_LOOP('',(#12002,#12003,#12004,#12005));
#2695=EDGE_LOOP('',(#12006,#12007,#12008,#12009));
#2696=EDGE_LOOP('',(#12010,#12011,#12012,#12013));
#2697=EDGE_LOOP('',(#12014,#12015,#12016,#12017));
#2698=EDGE_LOOP('',(#12018,#12019,#12020,#12021,#12022,#12023));
#2699=EDGE_LOOP('',(#12024,#12025,#12026));
#2700=EDGE_LOOP('',(#12027,#12028,#12029));
#2701=EDGE_LOOP('',(#12030,#12031,#12032,#12033,#12034,#12035));
#2702=EDGE_LOOP('',(#12036,#12037,#12038));
#2703=EDGE_LOOP('',(#12039,#12040,#12041));
#2704=EDGE_LOOP('',(#12042,#12043,#12044,#12045,#12046,#12047));
#2705=EDGE_LOOP('',(#12048,#12049,#12050));
#2706=EDGE_LOOP('',(#12051,#12052,#12053));
#2707=EDGE_LOOP('',(#12054,#12055,#12056,#12057));
#2708=EDGE_LOOP('',(#12058,#12059,#12060,#12061,#12062));
#2709=EDGE_LOOP('',(#12063,#12064));
#2710=EDGE_LOOP('',(#12065,#12066,#12067,#12068,#12069,#12070,#12071,#12072));
#2711=EDGE_LOOP('',(#12073,#12074));
#2712=EDGE_LOOP('',(#12075,#12076,#12077,#12078,#12079));
#2713=EDGE_LOOP('',(#12080,#12081,#12082,#12083,#12084));
#2714=EDGE_LOOP('',(#12085,#12086,#12087,#12088));
#2715=EDGE_LOOP('',(#12089,#12090,#12091,#12092,#12093));
#2716=EDGE_LOOP('',(#12094,#12095,#12096,#12097));
#2717=EDGE_LOOP('',(#12098,#12099,#12100,#12101));
#2718=EDGE_LOOP('',(#12102,#12103,#12104,#12105));
#2719=EDGE_LOOP('',(#12106,#12107,#12108,#12109,#12110));
#2720=EDGE_LOOP('',(#12111,#12112,#12113,#12114));
#2721=EDGE_LOOP('',(#12115,#12116,#12117,#12118));
#2722=EDGE_LOOP('',(#12119,#12120,#12121,#12122,#12123,#12124,#12125,#12126));
#2723=EDGE_LOOP('',(#12127,#12128,#12129,#12130,#12131,#12132,#12133,#12134));
#2724=EDGE_LOOP('',(#12135,#12136,#12137,#12138));
#2725=EDGE_LOOP('',(#12139,#12140,#12141,#12142,#12143,#12144));
#2726=EDGE_LOOP('',(#12145,#12146,#12147,#12148,#12149,#12150,#12151,#12152));
#2727=EDGE_LOOP('',(#12153,#12154,#12155,#12156,#12157,#12158,#12159,#12160,
#12161,#12162));
#2728=EDGE_LOOP('',(#12163,#12164,#12165,#12166));
#2729=EDGE_LOOP('',(#12167,#12168,#12169,#12170));
#2730=EDGE_LOOP('',(#12171,#12172,#12173,#12174));
#2731=EDGE_LOOP('',(#12175,#12176,#12177,#12178));
#2732=EDGE_LOOP('',(#12179,#12180,#12181,#12182));
#2733=EDGE_LOOP('',(#12183,#12184,#12185,#12186));
#2734=EDGE_LOOP('',(#12187,#12188,#12189,#12190));
#2735=EDGE_LOOP('',(#12191,#12192,#12193,#12194));
#2736=EDGE_LOOP('',(#12195,#12196,#12197,#12198));
#2737=EDGE_LOOP('',(#12199,#12200,#12201,#12202));
#2738=EDGE_LOOP('',(#12203,#12204,#12205,#12206));
#2739=EDGE_LOOP('',(#12207,#12208,#12209,#12210));
#2740=EDGE_LOOP('',(#12211,#12212,#12213,#12214));
#2741=EDGE_LOOP('',(#12215,#12216,#12217,#12218,#12219));
#2742=EDGE_LOOP('',(#12220,#12221,#12222,#12223));
#2743=EDGE_LOOP('',(#12224,#12225,#12226,#12227));
#2744=EDGE_LOOP('',(#12228,#12229,#12230,#12231));
#2745=EDGE_LOOP('',(#12232,#12233,#12234,#12235,#12236,#12237,#12238,#12239));
#2746=EDGE_LOOP('',(#12240,#12241,#12242,#12243,#12244));
#2747=EDGE_LOOP('',(#12245,#12246,#12247,#12248));
#2748=EDGE_LOOP('',(#12249,#12250,#12251,#12252,#12253));
#2749=EDGE_LOOP('',(#12254,#12255,#12256,#12257,#12258,#12259,#12260,#12261));
#2750=EDGE_LOOP('',(#12262,#12263,#12264,#12265));
#2751=EDGE_LOOP('',(#12266,#12267,#12268,#12269));
#2752=EDGE_LOOP('',(#12270,#12271,#12272,#12273));
#2753=EDGE_LOOP('',(#12274,#12275,#12276,#12277));
#2754=EDGE_LOOP('',(#12278,#12279,#12280,#12281,#12282,#12283));
#2755=EDGE_LOOP('',(#12284,#12285,#12286,#12287));
#2756=EDGE_LOOP('',(#12288,#12289,#12290,#12291));
#2757=EDGE_LOOP('',(#12292,#12293,#12294,#12295));
#2758=EDGE_LOOP('',(#12296,#12297,#12298,#12299,#12300,#12301));
#2759=EDGE_LOOP('',(#12302,#12303,#12304,#12305,#12306,#12307));
#2760=EDGE_LOOP('',(#12308,#12309,#12310));
#2761=EDGE_LOOP('',(#12311,#12312,#12313));
#2762=EDGE_LOOP('',(#12314,#12315,#12316,#12317));
#2763=EDGE_LOOP('',(#12318,#12319,#12320,#12321,#12322,#12323));
#2764=EDGE_LOOP('',(#12324,#12325,#12326,#12327,#12328,#12329,#12330));
#2765=EDGE_LOOP('',(#12331,#12332,#12333,#12334));
#2766=EDGE_LOOP('',(#12335,#12336,#12337,#12338,#12339,#12340));
#2767=EDGE_LOOP('',(#12341,#12342,#12343,#12344,#12345,#12346));
#2768=EDGE_LOOP('',(#12347,#12348,#12349,#12350));
#2769=EDGE_LOOP('',(#12351,#12352,#12353,#12354));
#2770=EDGE_LOOP('',(#12355,#12356,#12357,#12358));
#2771=EDGE_LOOP('',(#12359,#12360,#12361,#12362));
#2772=EDGE_LOOP('',(#12363,#12364,#12365,#12366));
#2773=EDGE_LOOP('',(#12367,#12368,#12369,#12370));
#2774=EDGE_LOOP('',(#12371,#12372,#12373,#12374));
#2775=EDGE_LOOP('',(#12375,#12376,#12377,#12378));
#2776=EDGE_LOOP('',(#12379,#12380,#12381,#12382,#12383));
#2777=EDGE_LOOP('',(#12384,#12385,#12386,#12387,#12388,#12389));
#2778=EDGE_LOOP('',(#12390,#12391,#12392));
#2779=EDGE_LOOP('',(#12393,#12394,#12395,#12396));
#2780=EDGE_LOOP('',(#12397,#12398,#12399,#12400));
#2781=EDGE_LOOP('',(#12401,#12402,#12403,#12404));
#2782=EDGE_LOOP('',(#12405,#12406,#12407,#12408,#12409,#12410,#12411,#12412,
#12413,#12414,#12415,#12416,#12417));
#2783=EDGE_LOOP('',(#12418,#12419,#12420,#12421,#12422,#12423,#12424,#12425,
#12426,#12427,#12428,#12429,#12430,#12431,#12432,#12433,#12434,#12435,#12436,
#12437,#12438,#12439,#12440,#12441,#12442,#12443,#12444,#12445,#12446,#12447,
#12448,#12449,#12450,#12451));
#2784=EDGE_LOOP('',(#12452,#12453,#12454,#12455,#12456,#12457,#12458,#12459));
#2785=EDGE_LOOP('',(#12460,#12461,#12462,#12463,#12464,#12465,#12466,#12467,
#12468,#12469,#12470,#12471,#12472,#12473,#12474,#12475,#12476,#12477,#12478,
#12479,#12480,#12481,#12482,#12483,#12484,#12485,#12486,#12487,#12488,#12489,
#12490,#12491,#12492,#12493,#12494,#12495,#12496,#12497));
#2786=EDGE_LOOP('',(#12498,#12499,#12500,#12501));
#2787=EDGE_LOOP('',(#12502,#12503,#12504,#12505,#12506,#12507,#12508,#12509));
#2788=EDGE_LOOP('',(#12510,#12511,#12512,#12513));
#2789=EDGE_LOOP('',(#12514,#12515,#12516,#12517));
#2790=EDGE_LOOP('',(#12518,#12519,#12520,#12521));
#2791=EDGE_LOOP('',(#12522,#12523,#12524,#12525));
#2792=EDGE_LOOP('',(#12526,#12527,#12528,#12529));
#2793=EDGE_LOOP('',(#12530,#12531,#12532,#12533,#12534,#12535,#12536));
#2794=EDGE_LOOP('',(#12537,#12538,#12539,#12540,#12541));
#2795=EDGE_LOOP('',(#12542,#12543,#12544,#12545));
#2796=EDGE_LOOP('',(#12546,#12547,#12548,#12549));
#2797=EDGE_LOOP('',(#12550,#12551,#12552,#12553,#12554,#12555));
#2798=EDGE_LOOP('',(#12556,#12557,#12558,#12559,#12560,#12561));
#2799=EDGE_LOOP('',(#12562,#12563,#12564));
#2800=EDGE_LOOP('',(#12565,#12566,#12567));
#2801=EDGE_LOOP('',(#12568,#12569,#12570,#12571));
#2802=EDGE_LOOP('',(#12572,#12573,#12574));
#2803=EDGE_LOOP('',(#12575,#12576,#12577,#12578));
#2804=EDGE_LOOP('',(#12579,#12580,#12581));
#2805=EDGE_LOOP('',(#12582,#12583,#12584,#12585));
#2806=EDGE_LOOP('',(#12586,#12587,#12588,#12589));
#2807=EDGE_LOOP('',(#12590,#12591,#12592));
#2808=EDGE_LOOP('',(#12593,#12594,#12595));
#2809=EDGE_LOOP('',(#12596,#12597,#12598,#12599));
#2810=EDGE_LOOP('',(#12600,#12601,#12602,#12603,#12604));
#2811=EDGE_LOOP('',(#12605,#12606,#12607,#12608,#12609));
#2812=EDGE_LOOP('',(#12610,#12611,#12612,#12613));
#2813=EDGE_LOOP('',(#12614,#12615,#12616,#12617,#12618));
#2814=EDGE_LOOP('',(#12619,#12620,#12621,#12622));
#2815=EDGE_LOOP('',(#12623,#12624,#12625,#12626));
#2816=EDGE_LOOP('',(#12627,#12628,#12629,#12630));
#2817=EDGE_LOOP('',(#12631,#12632,#12633,#12634));
#2818=EDGE_LOOP('',(#12635,#12636,#12637,#12638,#12639));
#2819=EDGE_LOOP('',(#12640,#12641,#12642,#12643,#12644,#12645,#12646,#12647,
#12648,#12649,#12650,#12651,#12652,#12653,#12654,#12655,#12656,#12657,#12658,
#12659,#12660,#12661,#12662,#12663,#12664,#12665,#12666,#12667,#12668,#12669,
#12670,#12671,#12672,#12673));
#2820=EDGE_LOOP('',(#12674,#12675,#12676,#12677,#12678,#12679,#12680,#12681,
#12682,#12683,#12684,#12685,#12686,#12687,#12688,#12689,#12690,#12691,#12692,
#12693,#12694,#12695,#12696,#12697,#12698));
#2821=EDGE_LOOP('',(#12699));
#2822=EDGE_LOOP('',(#12700));
#2823=EDGE_LOOP('',(#12701,#12702,#12703,#12704));
#2824=EDGE_LOOP('',(#12705));
#2825=EDGE_LOOP('',(#12706));
#2826=EDGE_LOOP('',(#12707,#12708,#12709,#12710,#12711));
#2827=EDGE_LOOP('',(#12712));
#2828=EDGE_LOOP('',(#12713));
#2829=EDGE_LOOP('',(#12714,#12715,#12716,#12717));
#2830=EDGE_LOOP('',(#12718,#12719,#12720,#12721,#12722));
#2831=EDGE_LOOP('',(#12723));
#2832=EDGE_LOOP('',(#12724));
#2833=EDGE_LOOP('',(#12725,#12726,#12727,#12728,#12729));
#2834=EDGE_LOOP('',(#12730,#12731,#12732,#12733));
#2835=EDGE_LOOP('',(#12734,#12735,#12736,#12737,#12738));
#2836=EDGE_LOOP('',(#12739,#12740,#12741,#12742));
#2837=EDGE_LOOP('',(#12743,#12744,#12745,#12746));
#2838=EDGE_LOOP('',(#12747,#12748,#12749,#12750,#12751));
#2839=EDGE_LOOP('',(#12752,#12753,#12754,#12755,#12756,#12757,#12758));
#2840=EDGE_LOOP('',(#12759,#12760,#12761,#12762,#12763));
#2841=EDGE_LOOP('',(#12764,#12765,#12766,#12767));
#2842=EDGE_LOOP('',(#12768,#12769,#12770,#12771));
#2843=EDGE_LOOP('',(#12772,#12773,#12774,#12775));
#2844=EDGE_LOOP('',(#12776,#12777,#12778,#12779));
#2845=EDGE_LOOP('',(#12780,#12781,#12782,#12783));
#2846=EDGE_LOOP('',(#12784,#12785,#12786,#12787,#12788,#12789,#12790));
#2847=EDGE_LOOP('',(#12791,#12792,#12793,#12794,#12795,#12796,#12797));
#2848=EDGE_LOOP('',(#12798,#12799,#12800,#12801,#12802));
#2849=EDGE_LOOP('',(#12803,#12804,#12805,#12806,#12807));
#2850=EDGE_LOOP('',(#12808,#12809,#12810,#12811));
#2851=EDGE_LOOP('',(#12812,#12813,#12814));
#2852=EDGE_LOOP('',(#12815,#12816,#12817,#12818));
#2853=EDGE_LOOP('',(#12819,#12820,#12821,#12822,#12823,#12824,#12825));
#2854=EDGE_LOOP('',(#12826,#12827,#12828,#12829));
#2855=EDGE_LOOP('',(#12830,#12831,#12832,#12833));
#2856=EDGE_LOOP('',(#12834,#12835,#12836,#12837));
#2857=EDGE_LOOP('',(#12838,#12839,#12840,#12841,#12842));
#2858=EDGE_LOOP('',(#12843,#12844,#12845,#12846));
#2859=EDGE_LOOP('',(#12847,#12848,#12849));
#2860=EDGE_LOOP('',(#12850,#12851,#12852,#12853));
#2861=EDGE_LOOP('',(#12854,#12855,#12856,#12857));
#2862=EDGE_LOOP('',(#12858,#12859,#12860,#12861,#12862,#12863,#12864));
#2863=EDGE_LOOP('',(#12865,#12866,#12867,#12868));
#2864=EDGE_LOOP('',(#12869,#12870,#12871,#12872,#12873));
#2865=EDGE_LOOP('',(#12874,#12875,#12876,#12877));
#2866=EDGE_LOOP('',(#12878,#12879,#12880,#12881));
#2867=EDGE_LOOP('',(#12882,#12883,#12884,#12885));
#2868=EDGE_LOOP('',(#12886,#12887,#12888));
#2869=EDGE_LOOP('',(#12889,#12890,#12891,#12892));
#2870=EDGE_LOOP('',(#12893,#12894,#12895,#12896,#12897,#12898,#12899));
#2871=EDGE_LOOP('',(#12900,#12901,#12902,#12903,#12904,#12905,#12906));
#2872=EDGE_LOOP('',(#12907,#12908,#12909,#12910,#12911));
#2873=EDGE_LOOP('',(#12912,#12913,#12914,#12915,#12916));
#2874=EDGE_LOOP('',(#12917,#12918,#12919,#12920));
#2875=EDGE_LOOP('',(#12921,#12922,#12923,#12924));
#2876=EDGE_LOOP('',(#12925,#12926,#12927,#12928));
#2877=EDGE_LOOP('',(#12929,#12930,#12931,#12932,#12933,#12934,#12935));
#2878=EDGE_LOOP('',(#12936,#12937,#12938,#12939));
#2879=EDGE_LOOP('',(#12940,#12941,#12942,#12943));
#2880=EDGE_LOOP('',(#12944,#12945,#12946,#12947));
#2881=EDGE_LOOP('',(#12948,#12949,#12950,#12951,#12952));
#2882=EDGE_LOOP('',(#12953,#12954,#12955,#12956));
#2883=EDGE_LOOP('',(#12957,#12958,#12959));
#2884=EDGE_LOOP('',(#12960,#12961,#12962,#12963));
#2885=EDGE_LOOP('',(#12964,#12965,#12966,#12967));
#2886=EDGE_LOOP('',(#12968,#12969,#12970,#12971,#12972,#12973,#12974));
#2887=EDGE_LOOP('',(#12975,#12976,#12977,#12978));
#2888=EDGE_LOOP('',(#12979,#12980,#12981,#12982,#12983));
#2889=EDGE_LOOP('',(#12984,#12985,#12986,#12987,#12988));
#2890=EDGE_LOOP('',(#12989,#12990,#12991,#12992));
#2891=EDGE_LOOP('',(#12993,#12994,#12995,#12996));
#2892=EDGE_LOOP('',(#12997,#12998,#12999,#13000));
#2893=EDGE_LOOP('',(#13001,#13002,#13003,#13004));
#2894=EDGE_LOOP('',(#13005,#13006,#13007,#13008,#13009,#13010,#13011));
#2895=EDGE_LOOP('',(#13012,#13013,#13014,#13015,#13016));
#2896=EDGE_LOOP('',(#13017,#13018,#13019,#13020));
#2897=EDGE_LOOP('',(#13021,#13022,#13023,#13024,#13025,#13026,#13027,#13028));
#2898=EDGE_LOOP('',(#13029,#13030,#13031,#13032));
#2899=EDGE_LOOP('',(#13033,#13034,#13035,#13036));
#2900=EDGE_LOOP('',(#13037,#13038,#13039,#13040,#13041,#13042,#13043,#13044));
#2901=EDGE_LOOP('',(#13045,#13046,#13047,#13048));
#2902=EDGE_LOOP('',(#13049,#13050,#13051,#13052));
#2903=EDGE_LOOP('',(#13053,#13054,#13055,#13056,#13057,#13058,#13059,#13060));
#2904=EDGE_LOOP('',(#13061,#13062,#13063,#13064));
#2905=EDGE_LOOP('',(#13065,#13066,#13067,#13068));
#2906=EDGE_LOOP('',(#13069,#13070,#13071,#13072,#13073,#13074,#13075,#13076));
#2907=EDGE_LOOP('',(#13077,#13078,#13079,#13080));
#2908=EDGE_LOOP('',(#13081,#13082,#13083,#13084));
#2909=EDGE_LOOP('',(#13085,#13086,#13087,#13088,#13089,#13090,#13091,#13092));
#2910=EDGE_LOOP('',(#13093,#13094,#13095,#13096));
#2911=EDGE_LOOP('',(#13097,#13098,#13099,#13100));
#2912=EDGE_LOOP('',(#13101));
#2913=EDGE_LOOP('',(#13102));
#2914=EDGE_LOOP('',(#13103,#13104,#13105,#13106));
#2915=EDGE_LOOP('',(#13107,#13108,#13109,#13110,#13111));
#2916=EDGE_LOOP('',(#13112,#13113,#13114,#13115,#13116,#13117,#13118,#13119,
#13120,#13121,#13122,#13123,#13124,#13125,#13126,#13127,#13128,#13129,#13130,
#13131,#13132,#13133,#13134,#13135,#13136));
#2917=EDGE_LOOP('',(#13137,#13138,#13139,#13140));
#2918=EDGE_LOOP('',(#13141,#13142,#13143,#13144,#13145,#13146,#13147,#13148,
#13149,#13150,#13151,#13152,#13153,#13154,#13155,#13156,#13157,#13158,#13159,
#13160,#13161,#13162,#13163,#13164));
#2919=EDGE_LOOP('',(#13165));
#2920=EDGE_LOOP('',(#13166));
#2921=EDGE_LOOP('',(#13167,#13168,#13169,#13170,#13171));
#2922=EDGE_LOOP('',(#13172,#13173,#13174,#13175));
#2923=EDGE_LOOP('',(#13176,#13177,#13178,#13179));
#2924=EDGE_LOOP('',(#13180,#13181,#13182,#13183));
#2925=EDGE_LOOP('',(#13184,#13185,#13186,#13187));
#2926=EDGE_LOOP('',(#13188,#13189,#13190,#13191));
#2927=EDGE_LOOP('',(#13192,#13193,#13194,#13195));
#2928=EDGE_LOOP('',(#13196,#13197,#13198,#13199));
#2929=EDGE_LOOP('',(#13200,#13201,#13202,#13203));
#2930=EDGE_LOOP('',(#13204,#13205,#13206,#13207));
#2931=EDGE_LOOP('',(#13208,#13209,#13210,#13211));
#2932=EDGE_LOOP('',(#13212,#13213,#13214,#13215,#13216));
#2933=EDGE_LOOP('',(#13217,#13218,#13219,#13220,#13221));
#2934=EDGE_LOOP('',(#13222,#13223,#13224,#13225,#13226));
#2935=EDGE_LOOP('',(#13227,#13228,#13229,#13230,#13231));
#2936=EDGE_LOOP('',(#13232,#13233,#13234,#13235,#13236));
#2937=EDGE_LOOP('',(#13237,#13238,#13239,#13240,#13241));
#2938=EDGE_LOOP('',(#13242,#13243,#13244,#13245,#13246));
#2939=EDGE_LOOP('',(#13247,#13248,#13249,#13250,#13251));
#2940=EDGE_LOOP('',(#13252,#13253,#13254,#13255,#13256));
#2941=EDGE_LOOP('',(#13257,#13258,#13259,#13260,#13261));
#2942=EDGE_LOOP('',(#13262,#13263,#13264,#13265,#13266));
#2943=EDGE_LOOP('',(#13267,#13268,#13269,#13270,#13271));
#2944=EDGE_LOOP('',(#13272,#13273,#13274,#13275,#13276));
#2945=EDGE_LOOP('',(#13277,#13278,#13279,#13280));
#2946=EDGE_LOOP('',(#13281,#13282,#13283,#13284,#13285,#13286,#13287,#13288,
#13289));
#2947=EDGE_LOOP('',(#13290,#13291,#13292,#13293));
#2948=EDGE_LOOP('',(#13294,#13295,#13296,#13297,#13298));
#2949=EDGE_LOOP('',(#13299,#13300,#13301,#13302));
#2950=EDGE_LOOP('',(#13303,#13304,#13305,#13306,#13307));
#2951=EDGE_LOOP('',(#13308,#13309,#13310,#13311));
#2952=EDGE_LOOP('',(#13312,#13313,#13314,#13315,#13316,#13317));
#2953=EDGE_LOOP('',(#13318,#13319,#13320,#13321));
#2954=EDGE_LOOP('',(#13322,#13323,#13324,#13325,#13326,#13327));
#2955=EDGE_LOOP('',(#13328,#13329,#13330,#13331,#13332,#13333,#13334,#13335));
#2956=EDGE_LOOP('',(#13336,#13337,#13338,#13339));
#2957=EDGE_LOOP('',(#13340,#13341,#13342,#13343));
#2958=EDGE_LOOP('',(#13344,#13345,#13346,#13347));
#2959=EDGE_LOOP('',(#13348,#13349,#13350,#13351));
#2960=EDGE_LOOP('',(#13352,#13353,#13354,#13355));
#2961=EDGE_LOOP('',(#13356,#13357,#13358,#13359));
#2962=EDGE_LOOP('',(#13360,#13361,#13362,#13363));
#2963=EDGE_LOOP('',(#13364,#13365,#13366,#13367,#13368));
#2964=EDGE_LOOP('',(#13369,#13370,#13371,#13372));
#2965=EDGE_LOOP('',(#13373,#13374,#13375,#13376,#13377));
#2966=EDGE_LOOP('',(#13378,#13379,#13380,#13381,#13382));
#2967=EDGE_LOOP('',(#13383,#13384,#13385,#13386,#13387));
#2968=EDGE_LOOP('',(#13388,#13389,#13390,#13391));
#2969=EDGE_LOOP('',(#13392,#13393,#13394,#13395));
#2970=EDGE_LOOP('',(#13396,#13397,#13398,#13399,#13400));
#2971=EDGE_LOOP('',(#13401,#13402,#13403,#13404,#13405));
#2972=EDGE_LOOP('',(#13406,#13407,#13408,#13409,#13410));
#2973=EDGE_LOOP('',(#13411,#13412,#13413,#13414,#13415));
#2974=EDGE_LOOP('',(#13416,#13417,#13418,#13419,#13420));
#2975=EDGE_LOOP('',(#13421,#13422,#13423,#13424,#13425));
#2976=EDGE_LOOP('',(#13426,#13427,#13428,#13429,#13430));
#2977=EDGE_LOOP('',(#13431,#13432,#13433,#13434,#13435));
#2978=EDGE_LOOP('',(#13436,#13437,#13438,#13439,#13440));
#2979=EDGE_LOOP('',(#13441,#13442,#13443,#13444));
#2980=EDGE_LOOP('',(#13445,#13446,#13447,#13448));
#2981=EDGE_LOOP('',(#13449,#13450,#13451,#13452));
#2982=EDGE_LOOP('',(#13453,#13454,#13455,#13456));
#2983=EDGE_LOOP('',(#13457,#13458,#13459,#13460));
#2984=EDGE_LOOP('',(#13461,#13462,#13463,#13464));
#2985=EDGE_LOOP('',(#13465,#13466,#13467,#13468));
#2986=EDGE_LOOP('',(#13469,#13470,#13471,#13472));
#2987=EDGE_LOOP('',(#13473,#13474,#13475,#13476));
#2988=EDGE_LOOP('',(#13477,#13478,#13479,#13480));
#2989=EDGE_LOOP('',(#13481,#13482,#13483,#13484));
#2990=EDGE_LOOP('',(#13485,#13486,#13487,#13488,#13489,#13490,#13491,#13492,
#13493,#13494,#13495,#13496));
#2991=EDGE_LOOP('',(#13497,#13498,#13499,#13500));
#2992=EDGE_LOOP('',(#13501,#13502,#13503,#13504,#13505,#13506,#13507,#13508,
#13509,#13510,#13511,#13512));
#2993=EDGE_LOOP('',(#13513,#13514,#13515,#13516));
#2994=EDGE_LOOP('',(#13517,#13518,#13519,#13520));
#2995=EDGE_LOOP('',(#13521,#13522,#13523,#13524,#13525));
#2996=EDGE_LOOP('',(#13526,#13527,#13528,#13529,#13530));
#2997=EDGE_LOOP('',(#13531,#13532,#13533,#13534,#13535));
#2998=EDGE_LOOP('',(#13536,#13537,#13538,#13539,#13540,#13541,#13542,#13543,
#13544,#13545,#13546,#13547,#13548,#13549,#13550,#13551,#13552,#13553,#13554,
#13555,#13556,#13557,#13558));
#2999=EDGE_LOOP('',(#13559));
#3000=EDGE_LOOP('',(#13560,#13561,#13562,#13563,#13564,#13565,#13566,#13567));
#3001=EDGE_LOOP('',(#13568));
#3002=EDGE_LOOP('',(#13569));
#3003=EDGE_LOOP('',(#13570));
#3004=EDGE_LOOP('',(#13571));
#3005=EDGE_LOOP('',(#13572));
#3006=EDGE_LOOP('',(#13573));
#3007=EDGE_LOOP('',(#13574));
#3008=EDGE_LOOP('',(#13575));
#3009=EDGE_LOOP('',(#13576));
#3010=EDGE_LOOP('',(#13577));
#3011=EDGE_LOOP('',(#13578));
#3012=EDGE_LOOP('',(#13579));
#3013=EDGE_LOOP('',(#13580));
#3014=EDGE_LOOP('',(#13581));
#3015=EDGE_LOOP('',(#13582));
#3016=EDGE_LOOP('',(#13583,#13584,#13585,#13586,#13587,#13588,#13589,#13590,
#13591,#13592,#13593,#13594,#13595,#13596,#13597,#13598,#13599,#13600,#13601,
#13602,#13603,#13604,#13605));
#3017=EDGE_LOOP('',(#13606,#13607,#13608,#13609,#13610,#13611,#13612,#13613));
#3018=EDGE_LOOP('',(#13614));
#3019=EDGE_LOOP('',(#13615));
#3020=EDGE_LOOP('',(#13616));
#3021=EDGE_LOOP('',(#13617));
#3022=EDGE_LOOP('',(#13618));
#3023=EDGE_LOOP('',(#13619));
#3024=EDGE_LOOP('',(#13620));
#3025=EDGE_LOOP('',(#13621));
#3026=EDGE_LOOP('',(#13622));
#3027=EDGE_LOOP('',(#13623));
#3028=EDGE_LOOP('',(#13624));
#3029=EDGE_LOOP('',(#13625));
#3030=EDGE_LOOP('',(#13626));
#3031=EDGE_LOOP('',(#13627));
#3032=EDGE_LOOP('',(#13628));
#3033=EDGE_LOOP('',(#13629));
#3034=EDGE_LOOP('',(#13630,#13631,#13632,#13633));
#3035=EDGE_LOOP('',(#13634,#13635,#13636,#13637));
#3036=EDGE_LOOP('',(#13638,#13639,#13640,#13641));
#3037=EDGE_LOOP('',(#13642,#13643,#13644,#13645));
#3038=EDGE_LOOP('',(#13646,#13647,#13648,#13649));
#3039=EDGE_LOOP('',(#13650,#13651,#13652,#13653,#13654));
#3040=EDGE_LOOP('',(#13655,#13656,#13657,#13658,#13659));
#3041=EDGE_LOOP('',(#13660,#13661,#13662,#13663,#13664));
#3042=EDGE_LOOP('',(#13665));
#3043=EDGE_LOOP('',(#13666,#13667,#13668,#13669,#13670));
#3044=EDGE_LOOP('',(#13671));
#3045=EDGE_LOOP('',(#13672,#13673,#13674,#13675,#13676));
#3046=EDGE_LOOP('',(#13677,#13678));
#3047=EDGE_LOOP('',(#13679,#13680,#13681,#13682));
#3048=EDGE_LOOP('',(#13683,#13684,#13685,#13686));
#3049=EDGE_LOOP('',(#13687));
#3050=EDGE_LOOP('',(#13688));
#3051=EDGE_LOOP('',(#13689,#13690,#13691,#13692));
#3052=EDGE_LOOP('',(#13693,#13694,#13695,#13696,#13697,#13698));
#3053=EDGE_LOOP('',(#13699,#13700,#13701,#13702,#13703,#13704,#13705,#13706,
#13707,#13708));
#3054=EDGE_LOOP('',(#13709,#13710,#13711,#13712,#13713));
#3055=EDGE_LOOP('',(#13714,#13715,#13716,#13717));
#3056=EDGE_LOOP('',(#13718,#13719,#13720,#13721));
#3057=EDGE_LOOP('',(#13722,#13723,#13724,#13725));
#3058=EDGE_LOOP('',(#13726,#13727,#13728,#13729));
#3059=EDGE_LOOP('',(#13730,#13731,#13732,#13733));
#3060=EDGE_LOOP('',(#13734,#13735,#13736,#13737));
#3061=EDGE_LOOP('',(#13738,#13739,#13740,#13741));
#3062=EDGE_LOOP('',(#13742,#13743,#13744,#13745));
#3063=EDGE_LOOP('',(#13746,#13747,#13748,#13749));
#3064=EDGE_LOOP('',(#13750,#13751,#13752,#13753));
#3065=EDGE_LOOP('',(#13754,#13755,#13756,#13757,#13758,#13759,#13760,#13761,
#13762,#13763,#13764));
#3066=EDGE_LOOP('',(#13765,#13766,#13767,#13768,#13769,#13770,#13771,#13772,
#13773,#13774,#13775));
#3067=EDGE_LOOP('',(#13776,#13777,#13778,#13779,#13780,#13781,#13782,#13783,
#13784,#13785,#13786,#13787));
#3068=EDGE_LOOP('',(#13788,#13789,#13790,#13791));
#3069=EDGE_LOOP('',(#13792,#13793,#13794,#13795));
#3070=EDGE_LOOP('',(#13796,#13797,#13798,#13799));
#3071=EDGE_LOOP('',(#13800,#13801,#13802,#13803));
#3072=EDGE_LOOP('',(#13804,#13805,#13806,#13807));
#3073=EDGE_LOOP('',(#13808,#13809,#13810,#13811,#13812,#13813));
#3074=EDGE_LOOP('',(#13814,#13815,#13816,#13817));
#3075=EDGE_LOOP('',(#13818,#13819,#13820,#13821,#13822,#13823,#13824,#13825,
#13826,#13827,#13828,#13829));
#3076=EDGE_LOOP('',(#13830,#13831,#13832,#13833));
#3077=EDGE_LOOP('',(#13834,#13835,#13836,#13837,#13838,#13839));
#3078=EDGE_LOOP('',(#13840,#13841,#13842,#13843));
#3079=EDGE_LOOP('',(#13844,#13845,#13846,#13847));
#3080=EDGE_LOOP('',(#13848,#13849,#13850,#13851));
#3081=EDGE_LOOP('',(#13852,#13853,#13854,#13855));
#3082=EDGE_LOOP('',(#13856,#13857,#13858,#13859));
#3083=EDGE_LOOP('',(#13860,#13861,#13862,#13863));
#3084=EDGE_LOOP('',(#13864,#13865,#13866,#13867));
#3085=EDGE_LOOP('',(#13868,#13869,#13870,#13871));
#3086=EDGE_LOOP('',(#13872,#13873,#13874,#13875));
#3087=EDGE_LOOP('',(#13876,#13877,#13878,#13879));
#3088=EDGE_LOOP('',(#13880,#13881,#13882,#13883));
#3089=EDGE_LOOP('',(#13884,#13885,#13886,#13887));
#3090=EDGE_LOOP('',(#13888,#13889,#13890,#13891));
#3091=EDGE_LOOP('',(#13892,#13893,#13894,#13895));
#3092=EDGE_LOOP('',(#13896,#13897,#13898,#13899));
#3093=EDGE_LOOP('',(#13900,#13901,#13902,#13903));
#3094=EDGE_LOOP('',(#13904,#13905,#13906,#13907));
#3095=EDGE_LOOP('',(#13908,#13909,#13910,#13911));
#3096=EDGE_LOOP('',(#13912,#13913,#13914,#13915));
#3097=EDGE_LOOP('',(#13916,#13917,#13918,#13919,#13920));
#3098=EDGE_LOOP('',(#13921,#13922,#13923,#13924));
#3099=EDGE_LOOP('',(#13925,#13926,#13927,#13928));
#3100=EDGE_LOOP('',(#13929,#13930,#13931,#13932));
#3101=EDGE_LOOP('',(#13933,#13934,#13935,#13936));
#3102=EDGE_LOOP('',(#13937,#13938,#13939,#13940));
#3103=EDGE_LOOP('',(#13941,#13942,#13943,#13944));
#3104=EDGE_LOOP('',(#13945,#13946,#13947,#13948));
#3105=EDGE_LOOP('',(#13949,#13950,#13951,#13952));
#3106=EDGE_LOOP('',(#13953,#13954,#13955,#13956));
#3107=EDGE_LOOP('',(#13957,#13958,#13959,#13960));
#3108=EDGE_LOOP('',(#13961,#13962,#13963,#13964));
#3109=EDGE_LOOP('',(#13965,#13966,#13967,#13968));
#3110=EDGE_LOOP('',(#13969,#13970,#13971,#13972));
#3111=EDGE_LOOP('',(#13973,#13974,#13975,#13976));
#3112=EDGE_LOOP('',(#13977,#13978,#13979,#13980));
#3113=EDGE_LOOP('',(#13981,#13982,#13983,#13984));
#3114=EDGE_LOOP('',(#13985,#13986,#13987,#13988));
#3115=EDGE_LOOP('',(#13989,#13990,#13991,#13992));
#3116=EDGE_LOOP('',(#13993,#13994,#13995,#13996));
#3117=EDGE_LOOP('',(#13997,#13998,#13999,#14000));
#3118=EDGE_LOOP('',(#14001,#14002,#14003,#14004));
#3119=EDGE_LOOP('',(#14005,#14006,#14007,#14008));
#3120=EDGE_LOOP('',(#14009,#14010,#14011,#14012));
#3121=EDGE_LOOP('',(#14013,#14014,#14015,#14016));
#3122=EDGE_LOOP('',(#14017,#14018,#14019,#14020));
#3123=EDGE_LOOP('',(#14021,#14022,#14023,#14024));
#3124=EDGE_LOOP('',(#14025,#14026,#14027,#14028));
#3125=EDGE_LOOP('',(#14029,#14030,#14031,#14032));
#3126=EDGE_LOOP('',(#14033,#14034,#14035,#14036));
#3127=EDGE_LOOP('',(#14037,#14038,#14039,#14040));
#3128=EDGE_LOOP('',(#14041,#14042,#14043,#14044));
#3129=EDGE_LOOP('',(#14045,#14046,#14047,#14048));
#3130=EDGE_LOOP('',(#14049,#14050,#14051,#14052));
#3131=EDGE_LOOP('',(#14053,#14054,#14055,#14056));
#3132=EDGE_LOOP('',(#14057,#14058,#14059,#14060));
#3133=EDGE_LOOP('',(#14061,#14062,#14063,#14064));
#3134=EDGE_LOOP('',(#14065,#14066,#14067,#14068));
#3135=EDGE_LOOP('',(#14069,#14070,#14071,#14072));
#3136=EDGE_LOOP('',(#14073,#14074,#14075,#14076,#14077));
#3137=EDGE_LOOP('',(#14078,#14079,#14080,#14081,#14082));
#3138=EDGE_LOOP('',(#14083,#14084,#14085,#14086));
#3139=EDGE_LOOP('',(#14087,#14088,#14089,#14090,#14091));
#3140=EDGE_LOOP('',(#14092,#14093,#14094,#14095));
#3141=EDGE_LOOP('',(#14096,#14097,#14098,#14099,#14100));
#3142=EDGE_LOOP('',(#14101,#14102,#14103,#14104));
#3143=EDGE_LOOP('',(#14105,#14106,#14107,#14108,#14109));
#3144=EDGE_LOOP('',(#14110,#14111,#14112,#14113));
#3145=EDGE_LOOP('',(#14114,#14115,#14116,#14117,#14118));
#3146=EDGE_LOOP('',(#14119,#14120,#14121,#14122,#14123));
#3147=EDGE_LOOP('',(#14124,#14125,#14126,#14127,#14128));
#3148=EDGE_LOOP('',(#14129,#14130,#14131,#14132,#14133));
#3149=EDGE_LOOP('',(#14134,#14135,#14136,#14137,#14138));
#3150=EDGE_LOOP('',(#14139,#14140,#14141,#14142));
#3151=EDGE_LOOP('',(#14143,#14144,#14145,#14146));
#3152=EDGE_LOOP('',(#14147,#14148,#14149,#14150,#14151,#14152,#14153,#14154,
#14155,#14156,#14157,#14158));
#3153=EDGE_LOOP('',(#14159));
#3154=EDGE_LOOP('',(#14160,#14161,#14162,#14163));
#3155=EDGE_LOOP('',(#14164,#14165,#14166,#14167));
#3156=EDGE_LOOP('',(#14168,#14169,#14170,#14171));
#3157=EDGE_LOOP('',(#14172,#14173,#14174,#14175,#14176,#14177,#14178,#14179,
#14180,#14181,#14182,#14183,#14184,#14185,#14186,#14187,#14188,#14189,#14190,
#14191));
#3158=EDGE_LOOP('',(#14192,#14193,#14194,#14195));
#3159=EDGE_LOOP('',(#14196,#14197,#14198,#14199));
#3160=EDGE_LOOP('',(#14200,#14201,#14202,#14203));
#3161=EDGE_LOOP('',(#14204,#14205,#14206,#14207));
#3162=EDGE_LOOP('',(#14208,#14209,#14210,#14211));
#3163=EDGE_LOOP('',(#14212,#14213,#14214,#14215));
#3164=EDGE_LOOP('',(#14216,#14217,#14218,#14219,#14220,#14221,#14222,#14223,
#14224,#14225,#14226,#14227,#14228,#14229,#14230,#14231,#14232,#14233,#14234,
#14235,#14236,#14237));
#3165=EDGE_LOOP('',(#14238,#14239,#14240,#14241,#14242,#14243,#14244,#14245,
#14246,#14247,#14248,#14249,#14250,#14251,#14252,#14253,#14254,#14255,#14256,
#14257,#14258));
#3166=EDGE_LOOP('',(#14259,#14260,#14261,#14262));
#3167=EDGE_LOOP('',(#14263));
#3168=EDGE_LOOP('',(#14264));
#3169=EDGE_LOOP('',(#14265,#14266,#14267,#14268));
#3170=EDGE_LOOP('',(#14269,#14270,#14271));
#3171=EDGE_LOOP('',(#14272,#14273,#14274,#14275));
#3172=EDGE_LOOP('',(#14276,#14277,#14278,#14279));
#3173=EDGE_LOOP('',(#14280,#14281,#14282,#14283));
#3174=EDGE_LOOP('',(#14284,#14285,#14286,#14287,#14288));
#3175=EDGE_LOOP('',(#14289,#14290,#14291,#14292));
#3176=EDGE_LOOP('',(#14293,#14294,#14295,#14296));
#3177=EDGE_LOOP('',(#14297));
#3178=EDGE_LOOP('',(#14298));
#3179=EDGE_LOOP('',(#14299));
#3180=EDGE_LOOP('',(#14300));
#3181=EDGE_LOOP('',(#14301,#14302,#14303,#14304,#14305,#14306,#14307,#14308,
#14309,#14310,#14311,#14312,#14313));
#3182=EDGE_LOOP('',(#14314));
#3183=EDGE_LOOP('',(#14315,#14316));
#3184=EDGE_LOOP('',(#14317,#14318,#14319,#14320));
#3185=EDGE_LOOP('',(#14321,#14322));
#3186=EDGE_LOOP('',(#14323,#14324));
#3187=EDGE_LOOP('',(#14325,#14326));
#3188=EDGE_LOOP('',(#14327,#14328,#14329,#14330,#14331,#14332));
#3189=EDGE_LOOP('',(#14333,#14334,#14335,#14336,#14337,#14338));
#3190=EDGE_LOOP('',(#14339,#14340,#14341,#14342,#14343,#14344));
#3191=EDGE_LOOP('',(#14345,#14346,#14347,#14348,#14349,#14350));
#3192=EDGE_LOOP('',(#14351,#14352,#14353,#14354));
#3193=EDGE_LOOP('',(#14355,#14356,#14357,#14358));
#3194=EDGE_LOOP('',(#14359,#14360,#14361,#14362));
#3195=EDGE_LOOP('',(#14363,#14364,#14365,#14366));
#3196=EDGE_LOOP('',(#14367,#14368,#14369,#14370));
#3197=EDGE_LOOP('',(#14371,#14372,#14373,#14374));
#3198=EDGE_LOOP('',(#14375,#14376,#14377,#14378));
#3199=EDGE_LOOP('',(#14379,#14380,#14381,#14382));
#3200=EDGE_LOOP('',(#14383,#14384,#14385,#14386));
#3201=EDGE_LOOP('',(#14387,#14388,#14389,#14390));
#3202=EDGE_LOOP('',(#14391,#14392,#14393,#14394));
#3203=EDGE_LOOP('',(#14395,#14396,#14397,#14398));
#3204=EDGE_LOOP('',(#14399,#14400,#14401,#14402));
#3205=EDGE_LOOP('',(#14403,#14404,#14405,#14406));
#3206=EDGE_LOOP('',(#14407,#14408,#14409,#14410));
#3207=EDGE_LOOP('',(#14411,#14412,#14413,#14414));
#3208=EDGE_LOOP('',(#14415,#14416,#14417,#14418));
#3209=EDGE_LOOP('',(#14419,#14420,#14421,#14422));
#3210=EDGE_LOOP('',(#14423,#14424,#14425,#14426));
#3211=EDGE_LOOP('',(#14427,#14428,#14429,#14430));
#3212=EDGE_LOOP('',(#14431,#14432,#14433,#14434));
#3213=EDGE_LOOP('',(#14435,#14436,#14437,#14438));
#3214=EDGE_LOOP('',(#14439,#14440,#14441,#14442));
#3215=EDGE_LOOP('',(#14443,#14444,#14445,#14446));
#3216=EDGE_LOOP('',(#14447,#14448,#14449,#14450));
#3217=EDGE_LOOP('',(#14451,#14452,#14453,#14454));
#3218=EDGE_LOOP('',(#14455,#14456,#14457,#14458));
#3219=EDGE_LOOP('',(#14459,#14460,#14461,#14462));
#3220=EDGE_LOOP('',(#14463,#14464,#14465,#14466));
#3221=EDGE_LOOP('',(#14467,#14468,#14469,#14470));
#3222=EDGE_LOOP('',(#14471,#14472,#14473,#14474));
#3223=EDGE_LOOP('',(#14475,#14476,#14477,#14478));
#3224=EDGE_LOOP('',(#14479,#14480,#14481,#14482));
#3225=EDGE_LOOP('',(#14483,#14484,#14485,#14486));
#3226=EDGE_LOOP('',(#14487,#14488,#14489,#14490));
#3227=EDGE_LOOP('',(#14491,#14492,#14493,#14494));
#3228=EDGE_LOOP('',(#14495,#14496,#14497,#14498));
#3229=EDGE_LOOP('',(#14499,#14500,#14501,#14502));
#3230=EDGE_LOOP('',(#14503,#14504,#14505,#14506));
#3231=EDGE_LOOP('',(#14507,#14508,#14509,#14510));
#3232=EDGE_LOOP('',(#14511,#14512,#14513,#14514));
#3233=EDGE_LOOP('',(#14515,#14516,#14517,#14518));
#3234=EDGE_LOOP('',(#14519,#14520,#14521,#14522));
#3235=EDGE_LOOP('',(#14523,#14524,#14525,#14526));
#3236=EDGE_LOOP('',(#14527,#14528,#14529,#14530));
#3237=EDGE_LOOP('',(#14531,#14532,#14533,#14534));
#3238=EDGE_LOOP('',(#14535,#14536,#14537,#14538));
#3239=EDGE_LOOP('',(#14539,#14540,#14541,#14542));
#3240=EDGE_LOOP('',(#14543,#14544,#14545,#14546));
#3241=EDGE_LOOP('',(#14547,#14548,#14549,#14550));
#3242=EDGE_LOOP('',(#14551,#14552,#14553,#14554));
#3243=EDGE_LOOP('',(#14555,#14556,#14557,#14558));
#3244=EDGE_LOOP('',(#14559,#14560,#14561,#14562));
#3245=EDGE_LOOP('',(#14563,#14564,#14565,#14566));
#3246=EDGE_LOOP('',(#14567,#14568,#14569,#14570));
#3247=EDGE_LOOP('',(#14571,#14572,#14573,#14574));
#3248=EDGE_LOOP('',(#14575,#14576,#14577,#14578));
#3249=EDGE_LOOP('',(#14579,#14580,#14581,#14582));
#3250=EDGE_LOOP('',(#14583,#14584,#14585,#14586));
#3251=EDGE_LOOP('',(#14587,#14588,#14589,#14590));
#3252=EDGE_LOOP('',(#14591,#14592,#14593,#14594));
#3253=EDGE_LOOP('',(#14595,#14596,#14597,#14598));
#3254=EDGE_LOOP('',(#14599,#14600,#14601,#14602));
#3255=EDGE_LOOP('',(#14603,#14604,#14605,#14606));
#3256=EDGE_LOOP('',(#14607,#14608,#14609,#14610));
#3257=EDGE_LOOP('',(#14611,#14612,#14613,#14614));
#3258=EDGE_LOOP('',(#14615,#14616,#14617,#14618));
#3259=EDGE_LOOP('',(#14619,#14620,#14621,#14622));
#3260=EDGE_LOOP('',(#14623,#14624,#14625,#14626));
#3261=EDGE_LOOP('',(#14627,#14628,#14629,#14630));
#3262=EDGE_LOOP('',(#14631,#14632,#14633,#14634));
#3263=EDGE_LOOP('',(#14635,#14636,#14637,#14638));
#3264=EDGE_LOOP('',(#14639,#14640,#14641,#14642));
#3265=EDGE_LOOP('',(#14643,#14644,#14645,#14646));
#3266=EDGE_LOOP('',(#14647,#14648,#14649,#14650));
#3267=EDGE_LOOP('',(#14651,#14652,#14653,#14654));
#3268=EDGE_LOOP('',(#14655,#14656,#14657,#14658));
#3269=EDGE_LOOP('',(#14659,#14660,#14661,#14662));
#3270=EDGE_LOOP('',(#14663,#14664,#14665,#14666));
#3271=EDGE_LOOP('',(#14667,#14668,#14669,#14670));
#3272=EDGE_LOOP('',(#14671,#14672,#14673,#14674));
#3273=EDGE_LOOP('',(#14675,#14676,#14677,#14678));
#3274=EDGE_LOOP('',(#14679,#14680,#14681,#14682));
#3275=EDGE_LOOP('',(#14683,#14684,#14685,#14686));
#3276=EDGE_LOOP('',(#14687,#14688,#14689,#14690));
#3277=EDGE_LOOP('',(#14691,#14692,#14693,#14694));
#3278=EDGE_LOOP('',(#14695,#14696,#14697,#14698));
#3279=EDGE_LOOP('',(#14699,#14700,#14701,#14702));
#3280=EDGE_LOOP('',(#14703,#14704,#14705,#14706));
#3281=EDGE_LOOP('',(#14707,#14708,#14709,#14710));
#3282=EDGE_LOOP('',(#14711,#14712,#14713,#14714));
#3283=EDGE_LOOP('',(#14715,#14716,#14717,#14718,#14719,#14720,#14721,#14722,
#14723,#14724,#14725,#14726,#14727,#14728,#14729,#14730,#14731,#14732,#14733,
#14734,#14735,#14736,#14737,#14738,#14739,#14740,#14741,#14742,#14743,#14744,
#14745,#14746,#14747,#14748,#14749,#14750,#14751,#14752,#14753,#14754,#14755,
#14756,#14757,#14758,#14759,#14760,#14761,#14762,#14763,#14764,#14765,#14766,
#14767,#14768,#14769,#14770,#14771,#14772,#14773,#14774,#14775,#14776,#14777,
#14778,#14779,#14780,#14781,#14782,#14783,#14784,#14785,#14786,#14787,#14788,
#14789,#14790,#14791,#14792,#14793,#14794,#14795,#14796,#14797,#14798,#14799,
#14800,#14801,#14802,#14803,#14804));
#3284=EDGE_LOOP('',(#14805));
#3285=EDGE_LOOP('',(#14806));
#3286=EDGE_LOOP('',(#14807));
#3287=EDGE_LOOP('',(#14808));
#3288=EDGE_LOOP('',(#14809));
#3289=EDGE_LOOP('',(#14810,#14811,#14812,#14813,#14814,#14815,#14816,#14817,
#14818,#14819,#14820,#14821,#14822,#14823,#14824,#14825,#14826,#14827,#14828,
#14829,#14830,#14831,#14832,#14833,#14834,#14835,#14836,#14837,#14838,#14839,
#14840,#14841,#14842,#14843,#14844,#14845,#14846,#14847,#14848,#14849,#14850,
#14851,#14852,#14853,#14854,#14855,#14856,#14857,#14858,#14859,#14860,#14861,
#14862,#14863,#14864,#14865,#14866,#14867,#14868,#14869,#14870,#14871,#14872,
#14873,#14874,#14875,#14876,#14877,#14878,#14879,#14880,#14881,#14882,#14883,
#14884,#14885,#14886,#14887,#14888,#14889,#14890,#14891,#14892,#14893,#14894,
#14895,#14896,#14897,#14898,#14899));
#3290=EDGE_LOOP('',(#14900,#14901,#14902,#14903,#14904,#14905,#14906,#14907,
#14908,#14909,#14910));
#3291=EDGE_LOOP('',(#14911,#14912,#14913,#14914));
#3292=EDGE_LOOP('',(#14915));
#3293=EDGE_LOOP('',(#14916));
#3294=EDGE_LOOP('',(#14917));
#3295=EDGE_LOOP('',(#14918));
#3296=EDGE_LOOP('',(#14919,#14920,#14921,#14922,#14923));
#3297=EDGE_LOOP('',(#14924,#14925,#14926,#14927,#14928,#14929,#14930,#14931,
#14932,#14933,#14934,#14935,#14936,#14937,#14938,#14939,#14940,#14941,#14942,
#14943,#14944,#14945,#14946,#14947,#14948,#14949,#14950,#14951,#14952,#14953,
#14954,#14955,#14956,#14957,#14958,#14959,#14960,#14961,#14962,#14963,#14964,
#14965,#14966,#14967));
#3298=EDGE_LOOP('',(#14968,#14969,#14970,#14971));
#3299=EDGE_LOOP('',(#14972,#14973,#14974,#14975,#14976,#14977,#14978,#14979,
#14980,#14981,#14982,#14983,#14984,#14985,#14986,#14987,#14988,#14989,#14990,
#14991,#14992,#14993,#14994,#14995,#14996,#14997,#14998,#14999,#15000,#15001,
#15002,#15003,#15004,#15005,#15006,#15007,#15008,#15009,#15010,#15011,#15012,
#15013,#15014,#15015,#15016));
#3300=EDGE_LOOP('',(#15017,#15018,#15019,#15020));
#3301=EDGE_LOOP('',(#15021,#15022,#15023,#15024,#15025));
#3302=EDGE_LOOP('',(#15026,#15027,#15028));
#3303=EDGE_LOOP('',(#15029,#15030,#15031));
#3304=EDGE_LOOP('',(#15032,#15033,#15034,#15035,#15036,#15037));
#3305=EDGE_LOOP('',(#15038,#15039,#15040,#15041,#15042));
#3306=EDGE_LOOP('',(#15043,#15044,#15045,#15046,#15047));
#3307=EDGE_LOOP('',(#15048,#15049,#15050,#15051));
#3308=EDGE_LOOP('',(#15052,#15053,#15054,#15055));
#3309=EDGE_LOOP('',(#15056));
#3310=EDGE_LOOP('',(#15057));
#3311=EDGE_LOOP('',(#15058));
#3312=EDGE_LOOP('',(#15059));
#3313=EDGE_LOOP('',(#15060,#15061,#15062,#15063));
#3314=EDGE_LOOP('',(#15064,#15065,#15066,#15067));
#3315=EDGE_LOOP('',(#15068,#15069,#15070));
#3316=EDGE_LOOP('',(#15071,#15072,#15073,#15074,#15075,#15076));
#3317=EDGE_LOOP('',(#15077,#15078,#15079,#15080,#15081,#15082));
#3318=EDGE_LOOP('',(#15083,#15084,#15085,#15086));
#3319=EDGE_LOOP('',(#15087,#15088,#15089,#15090));
#3320=EDGE_LOOP('',(#15091,#15092,#15093,#15094));
#3321=EDGE_LOOP('',(#15095,#15096,#15097,#15098));
#3322=EDGE_LOOP('',(#15099,#15100,#15101,#15102));
#3323=EDGE_LOOP('',(#15103,#15104,#15105,#15106));
#3324=EDGE_LOOP('',(#15107,#15108,#15109,#15110,#15111,#15112,#15113,#15114,
#15115,#15116,#15117,#15118));
#3325=EDGE_LOOP('',(#15119,#15120,#15121,#15122));
#3326=EDGE_LOOP('',(#15123,#15124,#15125,#15126));
#3327=EDGE_LOOP('',(#15127,#15128,#15129,#15130));
#3328=EDGE_LOOP('',(#15131,#15132,#15133,#15134));
#3329=EDGE_LOOP('',(#15135,#15136,#15137,#15138));
#3330=EDGE_LOOP('',(#15139,#15140,#15141,#15142));
#3331=EDGE_LOOP('',(#15143,#15144,#15145,#15146));
#3332=EDGE_LOOP('',(#15147,#15148,#15149,#15150));
#3333=EDGE_LOOP('',(#15151,#15152,#15153,#15154));
#3334=EDGE_LOOP('',(#15155,#15156,#15157,#15158));
#3335=EDGE_LOOP('',(#15159,#15160,#15161,#15162));
#3336=EDGE_LOOP('',(#15163,#15164,#15165,#15166));
#3337=EDGE_LOOP('',(#15167,#15168,#15169,#15170,#15171));
#3338=EDGE_LOOP('',(#15172,#15173,#15174,#15175));
#3339=EDGE_LOOP('',(#15176,#15177,#15178,#15179));
#3340=EDGE_LOOP('',(#15180,#15181,#15182,#15183));
#3341=EDGE_LOOP('',(#15184,#15185,#15186,#15187));
#3342=EDGE_LOOP('',(#15188,#15189,#15190,#15191,#15192));
#3343=EDGE_LOOP('',(#15193,#15194,#15195,#15196));
#3344=EDGE_LOOP('',(#15197,#15198,#15199,#15200,#15201,#15202));
#3345=EDGE_LOOP('',(#15203));
#3346=EDGE_LOOP('',(#15204));
#3347=EDGE_LOOP('',(#15205,#15206,#15207,#15208));
#3348=EDGE_LOOP('',(#15209,#15210,#15211,#15212));
#3349=EDGE_LOOP('',(#15213,#15214,#15215,#15216,#15217,#15218));
#3350=EDGE_LOOP('',(#15219,#15220,#15221,#15222));
#3351=EDGE_LOOP('',(#15223,#15224,#15225,#15226,#15227,#15228));
#3352=EDGE_LOOP('',(#15229,#15230,#15231,#15232));
#3353=EDGE_LOOP('',(#15233,#15234,#15235,#15236));
#3354=EDGE_LOOP('',(#15237));
#3355=EDGE_LOOP('',(#15238));
#3356=EDGE_LOOP('',(#15239,#15240,#15241,#15242));
#3357=EDGE_LOOP('',(#15243,#15244,#15245,#15246));
#3358=EDGE_LOOP('',(#15247));
#3359=EDGE_LOOP('',(#15248));
#3360=EDGE_LOOP('',(#15249,#15250,#15251,#15252));
#3361=EDGE_LOOP('',(#15253));
#3362=EDGE_LOOP('',(#15254));
#3363=EDGE_LOOP('',(#15255,#15256,#15257,#15258,#15259,#15260,#15261,#15262));
#3364=EDGE_LOOP('',(#15263,#15264,#15265,#15266));
#3365=EDGE_LOOP('',(#15267,#15268,#15269,#15270));
#3366=EDGE_LOOP('',(#15271,#15272,#15273,#15274));
#3367=EDGE_LOOP('',(#15275,#15276));
#3368=EDGE_LOOP('',(#15277,#15278,#15279,#15280,#15281,#15282,#15283,#15284));
#3369=EDGE_LOOP('',(#15285,#15286,#15287,#15288,#15289,#15290,#15291,#15292));
#3370=EDGE_LOOP('',(#15293));
#3371=EDGE_LOOP('',(#15294));
#3372=EDGE_LOOP('',(#15295));
#3373=EDGE_LOOP('',(#15296));
#3374=EDGE_LOOP('',(#15297,#15298,#15299,#15300));
#3375=EDGE_LOOP('',(#15301,#15302,#15303,#15304));
#3376=EDGE_LOOP('',(#15305,#15306,#15307,#15308,#15309,#15310));
#3377=EDGE_LOOP('',(#15311,#15312,#15313,#15314));
#3378=EDGE_LOOP('',(#15315,#15316,#15317,#15318,#15319,#15320));
#3379=EDGE_LOOP('',(#15321,#15322,#15323,#15324));
#3380=EDGE_LOOP('',(#15325,#15326,#15327,#15328));
#3381=EDGE_LOOP('',(#15329));
#3382=EDGE_LOOP('',(#15330));
#3383=EDGE_LOOP('',(#15331,#15332,#15333,#15334));
#3384=EDGE_LOOP('',(#15335,#15336,#15337,#15338,#15339,#15340));
#3385=EDGE_LOOP('',(#15341,#15342,#15343,#15344,#15345,#15346,#15347,#15348));
#3386=EDGE_LOOP('',(#15349,#15350,#15351,#15352,#15353,#15354,#15355,#15356));
#3387=EDGE_LOOP('',(#15357));
#3388=EDGE_LOOP('',(#15358,#15359,#15360,#15361,#15362,#15363,#15364,#15365,
#15366,#15367,#15368,#15369,#15370,#15371,#15372,#15373,#15374,#15375));
#3389=EDGE_LOOP('',(#15376,#15377,#15378,#15379));
#3390=EDGE_LOOP('',(#15380,#15381,#15382,#15383,#15384,#15385,#15386,#15387));
#3391=EDGE_LOOP('',(#15388,#15389,#15390,#15391,#15392,#15393,#15394,#15395));
#3392=EDGE_LOOP('',(#15396,#15397,#15398,#15399));
#3393=EDGE_LOOP('',(#15400,#15401,#15402,#15403));
#3394=EDGE_LOOP('',(#15404,#15405,#15406,#15407,#15408,#15409));
#3395=EDGE_LOOP('',(#15410,#15411,#15412,#15413));
#3396=EDGE_LOOP('',(#15414,#15415,#15416,#15417,#15418,#15419));
#3397=EDGE_LOOP('',(#15420,#15421,#15422,#15423,#15424,#15425,#15426,#15427,
#15428,#15429,#15430,#15431));
#3398=EDGE_LOOP('',(#15432));
#3399=EDGE_LOOP('',(#15433));
#3400=EDGE_LOOP('',(#15434,#15435,#15436,#15437,#15438));
#3401=EDGE_LOOP('',(#15439,#15440,#15441,#15442,#15443));
#3402=EDGE_LOOP('',(#15444,#15445,#15446,#15447));
#3403=EDGE_LOOP('',(#15448,#15449,#15450,#15451));
#3404=EDGE_LOOP('',(#15452,#15453,#15454,#15455));
#3405=EDGE_LOOP('',(#15456,#15457,#15458,#15459));
#3406=EDGE_LOOP('',(#15460,#15461,#15462,#15463));
#3407=EDGE_LOOP('',(#15464,#15465,#15466,#15467));
#3408=EDGE_LOOP('',(#15468,#15469,#15470,#15471));
#3409=EDGE_LOOP('',(#15472,#15473,#15474,#15475));
#3410=EDGE_LOOP('',(#15476,#15477,#15478,#15479));
#3411=EDGE_LOOP('',(#15480,#15481,#15482,#15483));
#3412=EDGE_LOOP('',(#15484,#15485,#15486,#15487));
#3413=EDGE_LOOP('',(#15488,#15489,#15490,#15491));
#3414=EDGE_LOOP('',(#15492,#15493,#15494,#15495));
#3415=EDGE_LOOP('',(#15496,#15497,#15498));
#3416=EDGE_LOOP('',(#15499,#15500,#15501,#15502));
#3417=EDGE_LOOP('',(#15503,#15504,#15505,#15506));
#3418=EDGE_LOOP('',(#15507,#15508,#15509,#15510));
#3419=EDGE_LOOP('',(#15511,#15512,#15513,#15514));
#3420=EDGE_LOOP('',(#15515,#15516,#15517,#15518));
#3421=EDGE_LOOP('',(#15519,#15520,#15521,#15522));
#3422=EDGE_LOOP('',(#15523,#15524,#15525,#15526));
#3423=EDGE_LOOP('',(#15527,#15528,#15529,#15530));
#3424=EDGE_LOOP('',(#15531,#15532,#15533,#15534));
#3425=EDGE_LOOP('',(#15535,#15536,#15537,#15538));
#3426=EDGE_LOOP('',(#15539,#15540,#15541,#15542));
#3427=EDGE_LOOP('',(#15543,#15544,#15545,#15546));
#3428=EDGE_LOOP('',(#15547,#15548,#15549,#15550));
#3429=EDGE_LOOP('',(#15551,#15552,#15553,#15554));
#3430=EDGE_LOOP('',(#15555,#15556,#15557,#15558));
#3431=EDGE_LOOP('',(#15559,#15560,#15561,#15562));
#3432=EDGE_LOOP('',(#15563,#15564,#15565,#15566));
#3433=EDGE_LOOP('',(#15567,#15568,#15569,#15570,#15571));
#3434=EDGE_LOOP('',(#15572,#15573,#15574,#15575,#15576));
#3435=EDGE_LOOP('',(#15577,#15578,#15579,#15580,#15581));
#3436=EDGE_LOOP('',(#15582,#15583,#15584,#15585,#15586));
#3437=EDGE_LOOP('',(#15587,#15588,#15589,#15590,#15591,#15592));
#3438=EDGE_LOOP('',(#15593,#15594,#15595,#15596,#15597,#15598));
#3439=EDGE_LOOP('',(#15599));
#3440=EDGE_LOOP('',(#15600));
#3441=EDGE_LOOP('',(#15601));
#3442=EDGE_LOOP('',(#15602));
#3443=EDGE_LOOP('',(#15603));
#3444=EDGE_LOOP('',(#15604));
#3445=EDGE_LOOP('',(#15605,#15606,#15607,#15608));
#3446=EDGE_LOOP('',(#15609,#15610,#15611,#15612,#15613,#15614,#15615,#15616,
#15617,#15618,#15619,#15620,#15621,#15622,#15623,#15624,#15625,#15626,#15627,
#15628,#15629,#15630,#15631,#15632,#15633,#15634,#15635,#15636,#15637,#15638,
#15639,#15640));
#3447=EDGE_LOOP('',(#15641,#15642,#15643,#15644));
#3448=EDGE_LOOP('',(#15645,#15646,#15647,#15648,#15649,#15650,#15651,#15652,
#15653,#15654,#15655,#15656,#15657,#15658,#15659,#15660,#15661,#15662,#15663,
#15664,#15665,#15666,#15667,#15668,#15669,#15670,#15671,#15672,#15673,#15674,
#15675,#15676));
#3449=EDGE_LOOP('',(#15677,#15678,#15679,#15680,#15681));
#3450=EDGE_LOOP('',(#15682,#15683,#15684,#15685));
#3451=EDGE_LOOP('',(#15686,#15687,#15688));
#3452=EDGE_LOOP('',(#15689,#15690,#15691,#15692,#15693,#15694));
#3453=EDGE_LOOP('',(#15695,#15696,#15697,#15698,#15699));
#3454=EDGE_LOOP('',(#15700,#15701,#15702,#15703,#15704));
#3455=EDGE_LOOP('',(#15705));
#3456=EDGE_LOOP('',(#15706));
#3457=EDGE_LOOP('',(#15707,#15708,#15709,#15710));
#3458=EDGE_LOOP('',(#15711));
#3459=EDGE_LOOP('',(#15712,#15713,#15714,#15715));
#3460=EDGE_LOOP('',(#15716,#15717,#15718,#15719));
#3461=EDGE_LOOP('',(#15720,#15721,#15722,#15723));
#3462=EDGE_LOOP('',(#15724,#15725,#15726,#15727));
#3463=EDGE_LOOP('',(#15728,#15729,#15730,#15731));
#3464=EDGE_LOOP('',(#15732,#15733,#15734,#15735));
#3465=EDGE_LOOP('',(#15736,#15737,#15738,#15739,#15740,#15741,#15742,#15743,
#15744,#15745,#15746,#15747,#15748,#15749));
#3466=EDGE_LOOP('',(#15750));
#3467=EDGE_LOOP('',(#15751));
#3468=EDGE_LOOP('',(#15752,#15753,#15754,#15755));
#3469=EDGE_LOOP('',(#15756,#15757,#15758,#15759,#15760,#15761,#15762,#15763,
#15764,#15765,#15766,#15767,#15768,#15769));
#3470=EDGE_LOOP('',(#15770));
#3471=EDGE_LOOP('',(#15771,#15772,#15773,#15774,#15775,#15776));
#3472=EDGE_LOOP('',(#15777,#15778,#15779,#15780,#15781,#15782,#15783,#15784,
#15785,#15786,#15787,#15788));
#3473=EDGE_LOOP('',(#15789,#15790,#15791,#15792));
#3474=EDGE_LOOP('',(#15793,#15794,#15795,#15796));
#3475=EDGE_LOOP('',(#15797,#15798,#15799,#15800));
#3476=EDGE_LOOP('',(#15801,#15802,#15803,#15804));
#3477=EDGE_LOOP('',(#15805,#15806,#15807,#15808));
#3478=EDGE_LOOP('',(#15809,#15810,#15811,#15812));
#3479=EDGE_LOOP('',(#15813,#15814,#15815,#15816));
#3480=EDGE_LOOP('',(#15817,#15818,#15819,#15820));
#3481=EDGE_LOOP('',(#15821,#15822,#15823,#15824,#15825,#15826,#15827,#15828,
#15829,#15830,#15831,#15832));
#3482=EDGE_LOOP('',(#15833,#15834,#15835,#15836,#15837,#15838,#15839,#15840,
#15841,#15842,#15843,#15844));
#3483=EDGE_LOOP('',(#15845,#15846,#15847,#15848,#15849,#15850,#15851,#15852,
#15853,#15854,#15855,#15856));
#3484=EDGE_LOOP('',(#15857,#15858,#15859,#15860));
#3485=EDGE_LOOP('',(#15861,#15862,#15863,#15864));
#3486=EDGE_LOOP('',(#15865,#15866,#15867,#15868));
#3487=EDGE_LOOP('',(#15869,#15870,#15871,#15872));
#3488=EDGE_LOOP('',(#15873));
#3489=EDGE_LOOP('',(#15874,#15875,#15876,#15877));
#3490=EDGE_LOOP('',(#15878,#15879,#15880,#15881));
#3491=EDGE_LOOP('',(#15882,#15883,#15884,#15885));
#3492=EDGE_LOOP('',(#15886,#15887,#15888,#15889));
#3493=EDGE_LOOP('',(#15890,#15891,#15892,#15893));
#3494=EDGE_LOOP('',(#15894,#15895,#15896,#15897));
#3495=EDGE_LOOP('',(#15898,#15899,#15900,#15901));
#3496=EDGE_LOOP('',(#15902,#15903,#15904,#15905));
#3497=EDGE_LOOP('',(#15906));
#3498=EDGE_LOOP('',(#15907,#15908,#15909,#15910));
#3499=EDGE_LOOP('',(#15911,#15912,#15913,#15914));
#3500=EDGE_LOOP('',(#15915,#15916,#15917,#15918));
#3501=EDGE_LOOP('',(#15919,#15920,#15921,#15922));
#3502=EDGE_LOOP('',(#15923));
#3503=EDGE_LOOP('',(#15924));
#3504=EDGE_LOOP('',(#15925));
#3505=EDGE_LOOP('',(#15926,#15927,#15928,#15929));
#3506=EDGE_LOOP('',(#15930,#15931,#15932,#15933));
#3507=EDGE_LOOP('',(#15934,#15935,#15936,#15937));
#3508=EDGE_LOOP('',(#15938,#15939,#15940,#15941));
#3509=EDGE_LOOP('',(#15942,#15943,#15944,#15945));
#3510=EDGE_LOOP('',(#15946,#15947,#15948,#15949));
#3511=EDGE_LOOP('',(#15950,#15951,#15952,#15953,#15954,#15955));
#3512=EDGE_LOOP('',(#15956,#15957,#15958,#15959));
#3513=EDGE_LOOP('',(#15960,#15961,#15962,#15963));
#3514=EDGE_LOOP('',(#15964,#15965,#15966,#15967));
#3515=EDGE_LOOP('',(#15968,#15969,#15970,#15971));
#3516=EDGE_LOOP('',(#15972,#15973,#15974,#15975));
#3517=EDGE_LOOP('',(#15976,#15977,#15978,#15979));
#3518=EDGE_LOOP('',(#15980,#15981,#15982,#15983,#15984));
#3519=EDGE_LOOP('',(#15985));
#3520=EDGE_LOOP('',(#15986));
#3521=EDGE_LOOP('',(#15987,#15988,#15989,#15990));
#3522=EDGE_LOOP('',(#15991,#15992,#15993,#15994));
#3523=EDGE_LOOP('',(#15995,#15996,#15997,#15998));
#3524=EDGE_LOOP('',(#15999,#16000,#16001,#16002));
#3525=EDGE_LOOP('',(#16003,#16004,#16005,#16006));
#3526=EDGE_LOOP('',(#16007,#16008,#16009,#16010));
#3527=EDGE_LOOP('',(#16011,#16012,#16013,#16014));
#3528=EDGE_LOOP('',(#16015,#16016,#16017,#16018));
#3529=EDGE_LOOP('',(#16019,#16020,#16021,#16022));
#3530=EDGE_LOOP('',(#16023,#16024,#16025,#16026));
#3531=EDGE_LOOP('',(#16027,#16028,#16029,#16030));
#3532=EDGE_LOOP('',(#16031,#16032,#16033,#16034));
#3533=EDGE_LOOP('',(#16035,#16036,#16037,#16038));
#3534=EDGE_LOOP('',(#16039,#16040,#16041,#16042));
#3535=EDGE_LOOP('',(#16043,#16044,#16045,#16046));
#3536=EDGE_LOOP('',(#16047,#16048,#16049,#16050));
#3537=EDGE_LOOP('',(#16051,#16052,#16053,#16054));
#3538=EDGE_LOOP('',(#16055,#16056,#16057,#16058));
#3539=EDGE_LOOP('',(#16059,#16060,#16061,#16062));
#3540=EDGE_LOOP('',(#16063,#16064,#16065,#16066));
#3541=EDGE_LOOP('',(#16067,#16068,#16069,#16070));
#3542=EDGE_LOOP('',(#16071,#16072,#16073,#16074));
#3543=EDGE_LOOP('',(#16075,#16076,#16077,#16078));
#3544=EDGE_LOOP('',(#16079,#16080,#16081,#16082));
#3545=EDGE_LOOP('',(#16083,#16084,#16085,#16086));
#3546=EDGE_LOOP('',(#16087,#16088,#16089,#16090));
#3547=EDGE_LOOP('',(#16091,#16092,#16093,#16094));
#3548=EDGE_LOOP('',(#16095,#16096,#16097,#16098));
#3549=EDGE_LOOP('',(#16099,#16100,#16101,#16102));
#3550=EDGE_LOOP('',(#16103,#16104,#16105,#16106));
#3551=EDGE_LOOP('',(#16107,#16108,#16109,#16110));
#3552=EDGE_LOOP('',(#16111,#16112,#16113,#16114));
#3553=EDGE_LOOP('',(#16115,#16116,#16117,#16118));
#3554=EDGE_LOOP('',(#16119,#16120,#16121,#16122));
#3555=EDGE_LOOP('',(#16123,#16124,#16125,#16126));
#3556=EDGE_LOOP('',(#16127,#16128,#16129,#16130));
#3557=EDGE_LOOP('',(#16131,#16132,#16133,#16134));
#3558=EDGE_LOOP('',(#16135,#16136,#16137,#16138));
#3559=EDGE_LOOP('',(#16139,#16140,#16141,#16142));
#3560=EDGE_LOOP('',(#16143,#16144,#16145,#16146));
#3561=EDGE_LOOP('',(#16147,#16148,#16149,#16150));
#3562=EDGE_LOOP('',(#16151,#16152,#16153,#16154));
#3563=EDGE_LOOP('',(#16155,#16156,#16157,#16158));
#3564=EDGE_LOOP('',(#16159,#16160,#16161,#16162));
#3565=EDGE_LOOP('',(#16163,#16164,#16165,#16166,#16167,#16168,#16169,#16170,
#16171,#16172,#16173,#16174,#16175,#16176,#16177,#16178,#16179,#16180,#16181,
#16182,#16183,#16184,#16185,#16186,#16187,#16188,#16189,#16190,#16191,#16192,
#16193,#16194,#16195,#16196,#16197,#16198,#16199,#16200,#16201,#16202,#16203,
#16204,#16205));
#3566=EDGE_LOOP('',(#16206));
#3567=EDGE_LOOP('',(#16207,#16208,#16209,#16210,#16211,#16212,#16213,#16214,
#16215,#16216,#16217,#16218,#16219,#16220,#16221,#16222,#16223,#16224,#16225,
#16226,#16227,#16228,#16229,#16230,#16231,#16232,#16233,#16234,#16235,#16236,
#16237,#16238,#16239,#16240,#16241,#16242,#16243,#16244,#16245,#16246,#16247,
#16248,#16249));
#3568=EDGE_LOOP('',(#16250));
#3569=EDGE_LOOP('',(#16251));
#3570=EDGE_LOOP('',(#16252,#16253,#16254,#16255));
#3571=EDGE_LOOP('',(#16256,#16257,#16258,#16259));
#3572=EDGE_LOOP('',(#16260,#16261,#16262,#16263));
#3573=EDGE_LOOP('',(#16264,#16265,#16266,#16267));
#3574=EDGE_LOOP('',(#16268,#16269,#16270,#16271));
#3575=EDGE_LOOP('',(#16272,#16273,#16274,#16275));
#3576=EDGE_LOOP('',(#16276,#16277,#16278,#16279));
#3577=EDGE_LOOP('',(#16280,#16281,#16282,#16283));
#3578=EDGE_LOOP('',(#16284,#16285,#16286,#16287));
#3579=EDGE_LOOP('',(#16288,#16289,#16290,#16291));
#3580=EDGE_LOOP('',(#16292,#16293,#16294,#16295));
#3581=EDGE_LOOP('',(#16296,#16297,#16298,#16299));
#3582=EDGE_LOOP('',(#16300,#16301,#16302,#16303,#16304,#16305,#16306,#16307,
#16308,#16309,#16310));
#3583=EDGE_LOOP('',(#16311));
#3584=EDGE_LOOP('',(#16312,#16313,#16314,#16315,#16316,#16317,#16318,#16319,
#16320,#16321,#16322));
#3585=EDGE_LOOP('',(#16323));
#3586=LINE('',#24199,#5296);
#3587=LINE('',#24201,#5297);
#3588=LINE('',#24203,#5298);
#3589=LINE('',#24204,#5299);
#3590=LINE('',#24259,#5300);
#3591=LINE('',#24261,#5301);
#3592=LINE('',#24263,#5302);
#3593=LINE('',#24264,#5303);
#3594=LINE('',#24267,#5304);
#3595=LINE('',#24269,#5305);
#3596=LINE('',#24271,#5306);
#3597=LINE('',#24272,#5307);
#3598=LINE('',#24275,#5308);
#3599=LINE('',#24277,#5309);
#3600=LINE('',#24279,#5310);
#3601=LINE('',#24280,#5311);
#3602=LINE('',#24283,#5312);
#3603=LINE('',#24285,#5313);
#3604=LINE('',#24287,#5314);
#3605=LINE('',#24288,#5315);
#3606=LINE('',#24291,#5316);
#3607=LINE('',#24293,#5317);
#3608=LINE('',#24295,#5318);
#3609=LINE('',#24296,#5319);
#3610=LINE('',#24299,#5320);
#3611=LINE('',#24301,#5321);
#3612=LINE('',#24303,#5322);
#3613=LINE('',#24304,#5323);
#3614=LINE('',#24307,#5324);
#3615=LINE('',#24309,#5325);
#3616=LINE('',#24311,#5326);
#3617=LINE('',#24312,#5327);
#3618=LINE('',#24315,#5328);
#3619=LINE('',#24317,#5329);
#3620=LINE('',#24319,#5330);
#3621=LINE('',#24320,#5331);
#3622=LINE('',#24323,#5332);
#3623=LINE('',#24325,#5333);
#3624=LINE('',#24327,#5334);
#3625=LINE('',#24328,#5335);
#3626=LINE('',#24331,#5336);
#3627=LINE('',#24333,#5337);
#3628=LINE('',#24335,#5338);
#3629=LINE('',#24336,#5339);
#3630=LINE('',#24339,#5340);
#3631=LINE('',#24341,#5341);
#3632=LINE('',#24343,#5342);
#3633=LINE('',#24344,#5343);
#3634=LINE('',#24347,#5344);
#3635=LINE('',#24349,#5345);
#3636=LINE('',#24351,#5346);
#3637=LINE('',#24352,#5347);
#3638=LINE('',#24355,#5348);
#3639=LINE('',#24357,#5349);
#3640=LINE('',#24359,#5350);
#3641=LINE('',#24360,#5351);
#3642=LINE('',#24363,#5352);
#3643=LINE('',#24365,#5353);
#3644=LINE('',#24367,#5354);
#3645=LINE('',#24368,#5355);
#3646=LINE('',#24371,#5356);
#3647=LINE('',#24373,#5357);
#3648=LINE('',#24375,#5358);
#3649=LINE('',#24376,#5359);
#3650=LINE('',#24379,#5360);
#3651=LINE('',#24381,#5361);
#3652=LINE('',#24383,#5362);
#3653=LINE('',#24384,#5363);
#3654=LINE('',#24387,#5364);
#3655=LINE('',#24389,#5365);
#3656=LINE('',#24391,#5366);
#3657=LINE('',#24392,#5367);
#3658=LINE('',#24395,#5368);
#3659=LINE('',#24397,#5369);
#3660=LINE('',#24399,#5370);
#3661=LINE('',#24400,#5371);
#3662=LINE('',#24403,#5372);
#3663=LINE('',#24405,#5373);
#3664=LINE('',#24407,#5374);
#3665=LINE('',#24408,#5375);
#3666=LINE('',#24411,#5376);
#3667=LINE('',#24413,#5377);
#3668=LINE('',#24415,#5378);
#3669=LINE('',#24416,#5379);
#3670=LINE('',#24419,#5380);
#3671=LINE('',#24421,#5381);
#3672=LINE('',#24423,#5382);
#3673=LINE('',#24424,#5383);
#3674=LINE('',#24427,#5384);
#3675=LINE('',#24429,#5385);
#3676=LINE('',#24431,#5386);
#3677=LINE('',#24432,#5387);
#3678=LINE('',#24435,#5388);
#3679=LINE('',#24437,#5389);
#3680=LINE('',#24439,#5390);
#3681=LINE('',#24440,#5391);
#3682=LINE('',#24443,#5392);
#3683=LINE('',#24445,#5393);
#3684=LINE('',#24447,#5394);
#3685=LINE('',#24448,#5395);
#3686=LINE('',#24451,#5396);
#3687=LINE('',#24453,#5397);
#3688=LINE('',#24455,#5398);
#3689=LINE('',#24456,#5399);
#3690=LINE('',#24459,#5400);
#3691=LINE('',#24461,#5401);
#3692=LINE('',#24463,#5402);
#3693=LINE('',#24464,#5403);
#3694=LINE('',#24468,#5404);
#3695=LINE('',#24470,#5405);
#3696=LINE('',#24472,#5406);
#3697=LINE('',#24473,#5407);
#3698=LINE('',#24476,#5408);
#3699=LINE('',#24478,#5409);
#3700=LINE('',#24480,#5410);
#3701=LINE('',#24481,#5411);
#3702=LINE('',#24484,#5412);
#3703=LINE('',#24486,#5413);
#3704=LINE('',#24488,#5414);
#3705=LINE('',#24489,#5415);
#3706=LINE('',#24492,#5416);
#3707=LINE('',#24494,#5417);
#3708=LINE('',#24496,#5418);
#3709=LINE('',#24497,#5419);
#3710=LINE('',#24500,#5420);
#3711=LINE('',#24502,#5421);
#3712=LINE('',#24504,#5422);
#3713=LINE('',#24505,#5423);
#3714=LINE('',#24508,#5424);
#3715=LINE('',#24510,#5425);
#3716=LINE('',#24512,#5426);
#3717=LINE('',#24513,#5427);
#3718=LINE('',#24516,#5428);
#3719=LINE('',#24518,#5429);
#3720=LINE('',#24520,#5430);
#3721=LINE('',#24521,#5431);
#3722=LINE('',#24524,#5432);
#3723=LINE('',#24526,#5433);
#3724=LINE('',#24528,#5434);
#3725=LINE('',#24529,#5435);
#3726=LINE('',#24532,#5436);
#3727=LINE('',#24534,#5437);
#3728=LINE('',#24536,#5438);
#3729=LINE('',#24537,#5439);
#3730=LINE('',#24540,#5440);
#3731=LINE('',#24542,#5441);
#3732=LINE('',#24544,#5442);
#3733=LINE('',#24545,#5443);
#3734=LINE('',#24548,#5444);
#3735=LINE('',#24550,#5445);
#3736=LINE('',#24552,#5446);
#3737=LINE('',#24553,#5447);
#3738=LINE('',#24556,#5448);
#3739=LINE('',#24558,#5449);
#3740=LINE('',#24560,#5450);
#3741=LINE('',#24561,#5451);
#3742=LINE('',#24564,#5452);
#3743=LINE('',#24566,#5453);
#3744=LINE('',#24568,#5454);
#3745=LINE('',#24569,#5455);
#3746=LINE('',#24572,#5456);
#3747=LINE('',#24574,#5457);
#3748=LINE('',#24576,#5458);
#3749=LINE('',#24577,#5459);
#3750=LINE('',#24580,#5460);
#3751=LINE('',#24582,#5461);
#3752=LINE('',#24584,#5462);
#3753=LINE('',#24585,#5463);
#3754=LINE('',#24588,#5464);
#3755=LINE('',#24590,#5465);
#3756=LINE('',#24592,#5466);
#3757=LINE('',#24593,#5467);
#3758=LINE('',#24596,#5468);
#3759=LINE('',#24598,#5469);
#3760=LINE('',#24600,#5470);
#3761=LINE('',#24601,#5471);
#3762=LINE('',#24604,#5472);
#3763=LINE('',#24606,#5473);
#3764=LINE('',#24608,#5474);
#3765=LINE('',#24609,#5475);
#3766=LINE('',#24612,#5476);
#3767=LINE('',#24614,#5477);
#3768=LINE('',#24616,#5478);
#3769=LINE('',#24617,#5479);
#3770=LINE('',#24620,#5480);
#3771=LINE('',#24622,#5481);
#3772=LINE('',#24624,#5482);
#3773=LINE('',#24625,#5483);
#3774=LINE('',#24628,#5484);
#3775=LINE('',#24630,#5485);
#3776=LINE('',#24632,#5486);
#3777=LINE('',#24633,#5487);
#3778=LINE('',#24636,#5488);
#3779=LINE('',#24638,#5489);
#3780=LINE('',#24640,#5490);
#3781=LINE('',#24641,#5491);
#3782=LINE('',#24644,#5492);
#3783=LINE('',#24646,#5493);
#3784=LINE('',#24648,#5494);
#3785=LINE('',#24649,#5495);
#3786=LINE('',#24652,#5496);
#3787=LINE('',#24654,#5497);
#3788=LINE('',#24656,#5498);
#3789=LINE('',#24657,#5499);
#3790=LINE('',#24660,#5500);
#3791=LINE('',#24662,#5501);
#3792=LINE('',#24664,#5502);
#3793=LINE('',#24665,#5503);
#3794=LINE('',#24668,#5504);
#3795=LINE('',#24670,#5505);
#3796=LINE('',#24672,#5506);
#3797=LINE('',#24673,#5507);
#3798=LINE('',#24676,#5508);
#3799=LINE('',#24678,#5509);
#3800=LINE('',#24680,#5510);
#3801=LINE('',#24681,#5511);
#3802=LINE('',#24735,#5512);
#3803=LINE('',#24736,#5513);
#3804=LINE('',#24738,#5514);
#3805=LINE('',#24740,#5515);
#3806=LINE('',#24742,#5516);
#3807=LINE('',#24744,#5517);
#3808=LINE('',#24746,#5518);
#3809=LINE('',#24748,#5519);
#3810=LINE('',#24750,#5520);
#3811=LINE('',#24752,#5521);
#3812=LINE('',#24754,#5522);
#3813=LINE('',#24756,#5523);
#3814=LINE('',#24758,#5524);
#3815=LINE('',#24760,#5525);
#3816=LINE('',#24762,#5526);
#3817=LINE('',#24764,#5527);
#3818=LINE('',#24766,#5528);
#3819=LINE('',#24768,#5529);
#3820=LINE('',#24770,#5530);
#3821=LINE('',#24772,#5531);
#3822=LINE('',#24774,#5532);
#3823=LINE('',#24776,#5533);
#3824=LINE('',#24778,#5534);
#3825=LINE('',#24780,#5535);
#3826=LINE('',#24782,#5536);
#3827=LINE('',#24784,#5537);
#3828=LINE('',#24786,#5538);
#3829=LINE('',#24788,#5539);
#3830=LINE('',#24790,#5540);
#3831=LINE('',#24791,#5541);
#3832=LINE('',#24793,#5542);
#3833=LINE('',#24794,#5543);
#3834=LINE('',#24796,#5544);
#3835=LINE('',#24797,#5545);
#3836=LINE('',#24799,#5546);
#3837=LINE('',#24800,#5547);
#3838=LINE('',#24802,#5548);
#3839=LINE('',#24803,#5549);
#3840=LINE('',#24805,#5550);
#3841=LINE('',#24806,#5551);
#3842=LINE('',#24808,#5552);
#3843=LINE('',#24809,#5553);
#3844=LINE('',#24811,#5554);
#3845=LINE('',#24812,#5555);
#3846=LINE('',#24814,#5556);
#3847=LINE('',#24815,#5557);
#3848=LINE('',#24817,#5558);
#3849=LINE('',#24818,#5559);
#3850=LINE('',#24820,#5560);
#3851=LINE('',#24821,#5561);
#3852=LINE('',#24823,#5562);
#3853=LINE('',#24824,#5563);
#3854=LINE('',#24826,#5564);
#3855=LINE('',#24827,#5565);
#3856=LINE('',#24829,#5566);
#3857=LINE('',#24830,#5567);
#3858=LINE('',#24832,#5568);
#3859=LINE('',#24833,#5569);
#3860=LINE('',#24835,#5570);
#3861=LINE('',#24836,#5571);
#3862=LINE('',#24838,#5572);
#3863=LINE('',#24839,#5573);
#3864=LINE('',#24841,#5574);
#3865=LINE('',#24842,#5575);
#3866=LINE('',#24844,#5576);
#3867=LINE('',#24845,#5577);
#3868=LINE('',#24847,#5578);
#3869=LINE('',#24848,#5579);
#3870=LINE('',#24850,#5580);
#3871=LINE('',#24851,#5581);
#3872=LINE('',#24853,#5582);
#3873=LINE('',#24854,#5583);
#3874=LINE('',#24856,#5584);
#3875=LINE('',#24857,#5585);
#3876=LINE('',#24859,#5586);
#3877=LINE('',#24860,#5587);
#3878=LINE('',#24862,#5588);
#3879=LINE('',#24863,#5589);
#3880=LINE('',#24865,#5590);
#3881=LINE('',#24866,#5591);
#3882=LINE('',#24868,#5592);
#3883=LINE('',#24870,#5593);
#3884=LINE('',#24872,#5594);
#3885=LINE('',#24874,#5595);
#3886=LINE('',#24877,#5596);
#3887=LINE('',#24879,#5597);
#3888=LINE('',#24882,#5598);
#3889=LINE('',#24884,#5599);
#3890=LINE('',#24887,#5600);
#3891=LINE('',#24889,#5601);
#3892=LINE('',#24892,#5602);
#3893=LINE('',#24894,#5603);
#3894=LINE('',#24897,#5604);
#3895=LINE('',#24899,#5605);
#3896=LINE('',#24902,#5606);
#3897=LINE('',#24904,#5607);
#3898=LINE('',#24907,#5608);
#3899=LINE('',#24909,#5609);
#3900=LINE('',#24912,#5610);
#3901=LINE('',#24914,#5611);
#3902=LINE('',#24917,#5612);
#3903=LINE('',#24919,#5613);
#3904=LINE('',#24922,#5614);
#3905=LINE('',#24924,#5615);
#3906=LINE('',#24927,#5616);
#3907=LINE('',#24929,#5617);
#3908=LINE('',#24932,#5618);
#3909=LINE('',#24934,#5619);
#3910=LINE('',#24937,#5620);
#3911=LINE('',#24939,#5621);
#3912=LINE('',#24942,#5622);
#3913=LINE('',#24944,#5623);
#3914=LINE('',#24947,#5624);
#3915=LINE('',#24949,#5625);
#3916=LINE('',#24952,#5626);
#3917=LINE('',#24954,#5627);
#3918=LINE('',#24957,#5628);
#3919=LINE('',#24959,#5629);
#3920=LINE('',#24962,#5630);
#3921=LINE('',#24964,#5631);
#3922=LINE('',#24967,#5632);
#3923=LINE('',#24969,#5633);
#3924=LINE('',#24972,#5634);
#3925=LINE('',#24974,#5635);
#3926=LINE('',#24977,#5636);
#3927=LINE('',#24979,#5637);
#3928=LINE('',#24982,#5638);
#3929=LINE('',#24984,#5639);
#3930=LINE('',#24987,#5640);
#3931=LINE('',#24989,#5641);
#3932=LINE('',#24992,#5642);
#3933=LINE('',#24994,#5643);
#3934=LINE('',#24997,#5644);
#3935=LINE('',#24999,#5645);
#3936=LINE('',#25010,#5646);
#3937=LINE('',#25015,#5647);
#3938=LINE('',#25017,#5648);
#3939=LINE('',#25019,#5649);
#3940=LINE('',#25027,#5650);
#3941=LINE('',#25032,#5651);
#3942=LINE('',#25034,#5652);
#3943=LINE('',#25036,#5653);
#3944=LINE('',#25044,#5654);
#3945=LINE('',#25049,#5655);
#3946=LINE('',#25051,#5656);
#3947=LINE('',#25053,#5657);
#3948=LINE('',#25076,#5658);
#3949=LINE('',#25078,#5659);
#3950=LINE('',#25086,#5660);
#3951=LINE('',#25088,#5661);
#3952=LINE('',#25089,#5662);
#3953=LINE('',#25091,#5663);
#3954=LINE('',#25093,#5664);
#3955=LINE('',#25094,#5665);
#3956=LINE('',#25103,#5666);
#3957=LINE('',#25104,#5667);
#3958=LINE('',#25123,#5668);
#3959=LINE('',#25125,#5669);
#3960=LINE('',#25130,#5670);
#3961=LINE('',#25134,#5671);
#3962=LINE('',#25136,#5672);
#3963=LINE('',#25137,#5673);
#3964=LINE('',#25140,#5674);
#3965=LINE('',#25142,#5675);
#3966=LINE('',#25143,#5676);
#3967=LINE('',#25146,#5677);
#3968=LINE('',#25148,#5678);
#3969=LINE('',#25149,#5679);
#3970=LINE('',#25152,#5680);
#3971=LINE('',#25154,#5681);
#3972=LINE('',#25155,#5682);
#3973=LINE('',#25158,#5683);
#3974=LINE('',#25160,#5684);
#3975=LINE('',#25162,#5685);
#3976=LINE('',#25165,#5686);
#3977=LINE('',#25166,#5687);
#3978=LINE('',#25172,#5688);
#3979=LINE('',#25175,#5689);
#3980=LINE('',#25178,#5690);
#3981=LINE('',#25180,#5691);
#3982=LINE('',#25184,#5692);
#3983=LINE('',#25187,#5693);
#3984=LINE('',#25188,#5694);
#3985=LINE('',#25190,#5695);
#3986=LINE('',#25192,#5696);
#3987=LINE('',#25193,#5697);
#3988=LINE('',#25195,#5698);
#3989=LINE('',#25197,#5699);
#3990=LINE('',#25199,#5700);
#3991=LINE('',#25201,#5701);
#3992=LINE('',#25202,#5702);
#3993=LINE('',#25209,#5703);
#3994=LINE('',#25212,#5704);
#3995=LINE('',#25218,#5705);
#3996=LINE('',#25221,#5706);
#3997=LINE('',#25227,#5707);
#3998=LINE('',#25230,#5708);
#3999=LINE('',#25236,#5709);
#4000=LINE('',#25239,#5710);
#4001=LINE('',#25243,#5711);
#4002=LINE('',#25245,#5712);
#4003=LINE('',#25247,#5713);
#4004=LINE('',#25248,#5714);
#4005=LINE('',#25251,#5715);
#4006=LINE('',#25253,#5716);
#4007=LINE('',#25254,#5717);
#4008=LINE('',#25257,#5718);
#4009=LINE('',#25259,#5719);
#4010=LINE('',#25260,#5720);
#4011=LINE('',#25263,#5721);
#4012=LINE('',#25265,#5722);
#4013=LINE('',#25266,#5723);
#4014=LINE('',#25269,#5724);
#4015=LINE('',#25271,#5725);
#4016=LINE('',#25272,#5726);
#4017=LINE('',#25275,#5727);
#4018=LINE('',#25277,#5728);
#4019=LINE('',#25278,#5729);
#4020=LINE('',#25281,#5730);
#4021=LINE('',#25283,#5731);
#4022=LINE('',#25284,#5732);
#4023=LINE('',#25288,#5733);
#4024=LINE('',#25290,#5734);
#4025=LINE('',#25292,#5735);
#4026=LINE('',#25293,#5736);
#4027=LINE('',#25297,#5737);
#4028=LINE('',#25299,#5738);
#4029=LINE('',#25301,#5739);
#4030=LINE('',#25302,#5740);
#4031=LINE('',#25305,#5741);
#4032=LINE('',#25306,#5742);
#4033=LINE('',#25307,#5743);
#4034=LINE('',#25310,#5744);
#4035=LINE('',#25312,#5745);
#4036=LINE('',#25313,#5746);
#4037=LINE('',#25315,#5747);
#4038=LINE('',#25316,#5748);
#4039=LINE('',#25318,#5749);
#4040=LINE('',#25319,#5750);
#4041=LINE('',#25322,#5751);
#4042=LINE('',#25324,#5752);
#4043=LINE('',#25325,#5753);
#4044=LINE('',#25328,#5754);
#4045=LINE('',#25329,#5755);
#4046=LINE('',#25330,#5756);
#4047=LINE('',#25332,#5757);
#4048=LINE('',#25335,#5758);
#4049=LINE('',#25336,#5759);
#4050=LINE('',#25338,#5760);
#4051=LINE('',#25340,#5761);
#4052=LINE('',#25341,#5762);
#4053=LINE('',#25347,#5763);
#4054=LINE('',#25350,#5764);
#4055=LINE('',#25356,#5765);
#4056=LINE('',#25359,#5766);
#4057=LINE('',#25364,#5767);
#4058=LINE('',#25366,#5768);
#4059=LINE('',#25370,#5769);
#4060=LINE('',#25373,#5770);
#4061=LINE('',#25375,#5771);
#4062=LINE('',#25376,#5772);
#4063=LINE('',#25377,#5773);
#4064=LINE('',#25378,#5774);
#4065=LINE('',#25380,#5775);
#4066=LINE('',#25381,#5776);
#4067=LINE('',#25384,#5777);
#4068=LINE('',#25385,#5778);
#4069=LINE('',#25387,#5779);
#4070=LINE('',#25391,#5780);
#4071=LINE('',#25392,#5781);
#4072=LINE('',#25395,#5782);
#4073=LINE('',#25396,#5783);
#4074=LINE('',#25400,#5784);
#4075=LINE('',#25402,#5785);
#4076=LINE('',#25404,#5786);
#4077=LINE('',#25405,#5787);
#4078=LINE('',#25409,#5788);
#4079=LINE('',#25411,#5789);
#4080=LINE('',#25415,#5790);
#4081=LINE('',#25417,#5791);
#4082=LINE('',#25422,#5792);
#4083=LINE('',#25424,#5793);
#4084=LINE('',#25426,#5794);
#4085=LINE('',#25427,#5795);
#4086=LINE('',#25431,#5796);
#4087=LINE('',#25433,#5797);
#4088=LINE('',#25437,#5798);
#4089=LINE('',#25439,#5799);
#4090=LINE('',#25445,#5800);
#4091=LINE('',#25449,#5801);
#4092=LINE('',#25454,#5802);
#4093=LINE('',#25455,#5803);
#4094=LINE('',#25456,#5804);
#4095=LINE('',#25460,#5805);
#4096=LINE('',#25464,#5806);
#4097=LINE('',#25465,#5807);
#4098=LINE('',#25469,#5808);
#4099=LINE('',#25473,#5809);
#4100=LINE('',#25478,#5810);
#4101=LINE('',#25479,#5811);
#4102=LINE('',#25480,#5812);
#4103=LINE('',#25484,#5813);
#4104=LINE('',#25488,#5814);
#4105=LINE('',#25489,#5815);
#4106=LINE('',#25495,#5816);
#4107=LINE('',#25497,#5817);
#4108=LINE('',#25499,#5818);
#4109=LINE('',#25500,#5819);
#4110=LINE('',#25502,#5820);
#4111=LINE('',#25504,#5821);
#4112=LINE('',#25505,#5822);
#4113=LINE('',#25508,#5823);
#4114=LINE('',#25512,#5824);
#4115=LINE('',#25514,#5825);
#4116=LINE('',#25515,#5826);
#4117=LINE('',#25517,#5827);
#4118=LINE('',#25518,#5828);
#4119=LINE('',#25522,#5829);
#4120=LINE('',#25523,#5830);
#4121=LINE('',#25524,#5831);
#4122=LINE('',#25525,#5832);
#4123=LINE('',#25528,#5833);
#4124=LINE('',#25529,#5834);
#4125=LINE('',#25531,#5835);
#4126=LINE('',#25532,#5836);
#4127=LINE('',#25533,#5837);
#4128=LINE('',#25534,#5838);
#4129=LINE('',#25535,#5839);
#4130=LINE('',#25536,#5840);
#4131=LINE('',#25537,#5841);
#4132=LINE('',#25539,#5842);
#4133=LINE('',#25541,#5843);
#4134=LINE('',#25543,#5844);
#4135=LINE('',#25545,#5845);
#4136=LINE('',#25546,#5846);
#4137=LINE('',#25548,#5847);
#4138=LINE('',#25742,#5848);
#4139=LINE('',#25745,#5849);
#4140=LINE('',#26011,#5850);
#4141=LINE('',#26154,#5851);
#4142=LINE('',#26157,#5852);
#4143=LINE('',#26162,#5853);
#4144=LINE('',#26164,#5854);
#4145=LINE('',#26190,#5855);
#4146=LINE('',#26193,#5856);
#4147=LINE('',#26203,#5857);
#4148=LINE('',#26220,#5858);
#4149=LINE('',#26221,#5859);
#4150=LINE('',#26241,#5860);
#4151=LINE('',#26243,#5861);
#4152=LINE('',#26295,#5862);
#4153=LINE('',#26296,#5863);
#4154=LINE('',#26299,#5864);
#4155=LINE('',#26301,#5865);
#4156=LINE('',#26319,#5866);
#4157=LINE('',#26321,#5867);
#4158=LINE('',#26323,#5868);
#4159=LINE('',#26324,#5869);
#4160=LINE('',#26329,#5870);
#4161=LINE('',#26332,#5871);
#4162=LINE('',#26337,#5872);
#4163=LINE('',#26339,#5873);
#4164=LINE('',#26401,#5874);
#4165=LINE('',#26403,#5875);
#4166=LINE('',#26404,#5876);
#4167=LINE('',#26410,#5877);
#4168=LINE('',#26411,#5878);
#4169=LINE('',#26420,#5879);
#4170=LINE('',#26422,#5880);
#4171=LINE('',#26432,#5881);
#4172=LINE('',#26433,#5882);
#4173=LINE('',#26438,#5883);
#4174=LINE('',#26455,#5884);
#4175=LINE('',#26456,#5885);
#4176=LINE('',#26458,#5886);
#4177=LINE('',#26459,#5887);
#4178=LINE('',#26479,#5888);
#4179=LINE('',#26481,#5889);
#4180=LINE('',#26536,#5890);
#4181=LINE('',#26537,#5891);
#4182=LINE('',#26540,#5892);
#4183=LINE('',#26542,#5893);
#4184=LINE('',#26560,#5894);
#4185=LINE('',#26562,#5895);
#4186=LINE('',#26566,#5896);
#4187=LINE('',#26567,#5897);
#4188=LINE('',#26569,#5898);
#4189=LINE('',#26572,#5899);
#4190=LINE('',#26577,#5900);
#4191=LINE('',#26579,#5901);
#4192=LINE('',#26643,#5902);
#4193=LINE('',#26645,#5903);
#4194=LINE('',#26646,#5904);
#4195=LINE('',#26650,#5905);
#4196=LINE('',#26651,#5906);
#4197=LINE('',#26660,#5907);
#4198=LINE('',#26662,#5908);
#4199=LINE('',#26672,#5909);
#4200=LINE('',#26673,#5910);
#4201=LINE('',#26680,#5911);
#4202=LINE('',#26697,#5912);
#4203=LINE('',#26698,#5913);
#4204=LINE('',#26700,#5914);
#4205=LINE('',#26701,#5915);
#4206=LINE('',#26721,#5916);
#4207=LINE('',#26723,#5917);
#4208=LINE('',#26777,#5918);
#4209=LINE('',#26778,#5919);
#4210=LINE('',#26780,#5920);
#4211=LINE('',#26782,#5921);
#4212=LINE('',#26783,#5922);
#4213=LINE('',#26787,#5923);
#4214=LINE('',#26788,#5924);
#4215=LINE('',#26796,#5925);
#4216=LINE('',#26797,#5926);
#4217=LINE('',#26801,#5927);
#4218=LINE('',#26802,#5928);
#4219=LINE('',#26806,#5929);
#4220=LINE('',#26807,#5930);
#4221=LINE('',#26811,#5931);
#4222=LINE('',#26812,#5932);
#4223=LINE('',#26816,#5933);
#4224=LINE('',#26817,#5934);
#4225=LINE('',#26828,#5935);
#4226=LINE('',#26830,#5936);
#4227=LINE('',#26833,#5937);
#4228=LINE('',#26836,#5938);
#4229=LINE('',#26847,#5939);
#4230=LINE('',#26850,#5940);
#4231=LINE('',#26856,#5941);
#4232=LINE('',#26859,#5942);
#4233=LINE('',#26865,#5943);
#4234=LINE('',#26868,#5944);
#4235=LINE('',#26874,#5945);
#4236=LINE('',#26877,#5946);
#4237=LINE('',#26883,#5947);
#4238=LINE('',#26886,#5948);
#4239=LINE('',#26892,#5949);
#4240=LINE('',#26895,#5950);
#4241=LINE('',#26902,#5951);
#4242=LINE('',#26910,#5952);
#4243=LINE('',#26918,#5953);
#4244=LINE('',#26926,#5954);
#4245=LINE('',#26934,#5955);
#4246=LINE('',#26942,#5956);
#4247=LINE('',#26950,#5957);
#4248=LINE('',#26958,#5958);
#4249=LINE('',#26966,#5959);
#4250=LINE('',#26974,#5960);
#4251=LINE('',#26982,#5961);
#4252=LINE('',#26990,#5962);
#4253=LINE('',#26998,#5963);
#4254=LINE('',#27003,#5964);
#4255=LINE('',#27005,#5965);
#4256=LINE('',#27007,#5966);
#4257=LINE('',#27008,#5967);
#4258=LINE('',#27014,#5968);
#4259=LINE('',#27016,#5969);
#4260=LINE('',#27020,#5970);
#4261=LINE('',#27024,#5971);
#4262=LINE('',#27026,#5972);
#4263=LINE('',#27027,#5973);
#4264=LINE('',#27031,#5974);
#4265=LINE('',#27033,#5975);
#4266=LINE('',#27035,#5976);
#4267=LINE('',#27036,#5977);
#4268=LINE('',#27040,#5978);
#4269=LINE('',#27041,#5979);
#4270=LINE('',#27043,#5980);
#4271=LINE('',#27044,#5981);
#4272=LINE('',#27047,#5982);
#4273=LINE('',#27048,#5983);
#4274=LINE('',#27051,#5984);
#4275=LINE('',#27053,#5985);
#4276=LINE('',#27054,#5986);
#4277=LINE('',#27057,#5987);
#4278=LINE('',#27059,#5988);
#4279=LINE('',#27062,#5989);
#4280=LINE('',#27064,#5990);
#4281=LINE('',#27067,#5991);
#4282=LINE('',#27073,#5992);
#4283=LINE('',#27076,#5993);
#4284=LINE('',#27078,#5994);
#4285=LINE('',#27080,#5995);
#4286=LINE('',#27083,#5996);
#4287=LINE('',#27086,#5997);
#4288=LINE('',#27088,#5998);
#4289=LINE('',#27090,#5999);
#4290=LINE('',#27091,#6000);
#4291=LINE('',#27093,#6001);
#4292=LINE('',#27094,#6002);
#4293=LINE('',#27096,#6003);
#4294=LINE('',#27098,#6004);
#4295=LINE('',#27101,#6005);
#4296=LINE('',#27102,#6006);
#4297=LINE('',#27104,#6007);
#4298=LINE('',#27105,#6008);
#4299=LINE('',#27107,#6009);
#4300=LINE('',#27108,#6010);
#4301=LINE('',#27110,#6011);
#4302=LINE('',#27111,#6012);
#4303=LINE('',#27114,#6013);
#4304=LINE('',#27120,#6014);
#4305=LINE('',#27124,#6015);
#4306=LINE('',#27128,#6016);
#4307=LINE('',#27132,#6017);
#4308=LINE('',#27138,#6018);
#4309=LINE('',#27144,#6019);
#4310=LINE('',#27148,#6020);
#4311=LINE('',#27152,#6021);
#4312=LINE('',#27156,#6022);
#4313=LINE('',#27160,#6023);
#4314=LINE('',#27164,#6024);
#4315=LINE('',#27168,#6025);
#4316=LINE('',#27172,#6026);
#4317=LINE('',#27176,#6027);
#4318=LINE('',#27180,#6028);
#4319=LINE('',#27185,#6029);
#4320=LINE('',#27187,#6030);
#4321=LINE('',#27189,#6031);
#4322=LINE('',#27190,#6032);
#4323=LINE('',#27193,#6033);
#4324=LINE('',#27195,#6034);
#4325=LINE('',#27196,#6035);
#4326=LINE('',#27198,#6036);
#4327=LINE('',#27199,#6037);
#4328=LINE('',#27202,#6038);
#4329=LINE('',#27204,#6039);
#4330=LINE('',#27205,#6040);
#4331=LINE('',#27211,#6041);
#4332=LINE('',#27213,#6042);
#4333=LINE('',#27214,#6043);
#4334=LINE('',#27217,#6044);
#4335=LINE('',#27219,#6045);
#4336=LINE('',#27220,#6046);
#4337=LINE('',#27226,#6047);
#4338=LINE('',#27229,#6048);
#4339=LINE('',#27231,#6049);
#4340=LINE('',#27232,#6050);
#4341=LINE('',#27238,#6051);
#4342=LINE('',#27241,#6052);
#4343=LINE('',#27243,#6053);
#4344=LINE('',#27244,#6054);
#4345=LINE('',#27246,#6055);
#4346=LINE('',#27248,#6056);
#4347=LINE('',#27249,#6057);
#4348=LINE('',#27250,#6058);
#4349=LINE('',#27252,#6059);
#4350=LINE('',#27253,#6060);
#4351=LINE('',#27256,#6061);
#4352=LINE('',#27257,#6062);
#4353=LINE('',#27260,#6063);
#4354=LINE('',#27262,#6064);
#4355=LINE('',#27264,#6065);
#4356=LINE('',#27265,#6066);
#4357=LINE('',#27267,#6067);
#4358=LINE('',#27268,#6068);
#4359=LINE('',#27271,#6069);
#4360=LINE('',#27273,#6070);
#4361=LINE('',#27274,#6071);
#4362=LINE('',#27277,#6072);
#4363=LINE('',#27279,#6073);
#4364=LINE('',#27280,#6074);
#4365=LINE('',#27282,#6075);
#4366=LINE('',#27283,#6076);
#4367=LINE('',#27285,#6077);
#4368=LINE('',#27287,#6078);
#4369=LINE('',#27288,#6079);
#4370=LINE('',#27292,#6080);
#4371=LINE('',#27294,#6081);
#4372=LINE('',#27302,#6082);
#4373=LINE('',#27305,#6083);
#4374=LINE('',#27311,#6084);
#4375=LINE('',#27314,#6085);
#4376=LINE('',#27317,#6086);
#4377=LINE('',#27318,#6087);
#4378=LINE('',#27319,#6088);
#4379=LINE('',#27392,#6089);
#4380=LINE('',#27397,#6090);
#4381=LINE('',#27399,#6091);
#4382=LINE('',#27403,#6092);
#4383=LINE('',#27405,#6093);
#4384=LINE('',#27407,#6094);
#4385=LINE('',#27408,#6095);
#4386=LINE('',#27412,#6096);
#4387=LINE('',#27413,#6097);
#4388=LINE('',#27414,#6098);
#4389=LINE('',#27417,#6099);
#4390=LINE('',#27418,#6100);
#4391=LINE('',#27420,#6101);
#4392=LINE('',#27421,#6102);
#4393=LINE('',#27423,#6103);
#4394=LINE('',#27429,#6104);
#4395=LINE('',#27431,#6105);
#4396=LINE('',#27433,#6106);
#4397=LINE('',#27434,#6107);
#4398=LINE('',#27438,#6108);
#4399=LINE('',#27440,#6109);
#4400=LINE('',#27442,#6110);
#4401=LINE('',#27443,#6111);
#4402=LINE('',#27449,#6112);
#4403=LINE('',#27452,#6113);
#4404=LINE('',#27458,#6114);
#4405=LINE('',#27461,#6115);
#4406=LINE('',#27467,#6116);
#4407=LINE('',#27470,#6117);
#4408=LINE('',#27476,#6118);
#4409=LINE('',#27479,#6119);
#4410=LINE('',#27482,#6120);
#4411=LINE('',#27484,#6121);
#4412=LINE('',#27485,#6122);
#4413=LINE('',#27487,#6123);
#4414=LINE('',#27488,#6124);
#4415=LINE('',#27491,#6125);
#4416=LINE('',#27493,#6126);
#4417=LINE('',#27494,#6127);
#4418=LINE('',#27496,#6128);
#4419=LINE('',#27497,#6129);
#4420=LINE('',#27500,#6130);
#4421=LINE('',#27501,#6131);
#4422=LINE('',#27503,#6132);
#4423=LINE('',#27505,#6133);
#4424=LINE('',#27507,#6134);
#4425=LINE('',#27509,#6135);
#4426=LINE('',#27511,#6136);
#4427=LINE('',#27513,#6137);
#4428=LINE('',#27514,#6138);
#4429=LINE('',#27517,#6139);
#4430=LINE('',#27518,#6140);
#4431=LINE('',#27520,#6141);
#4432=LINE('',#27522,#6142);
#4433=LINE('',#27524,#6143);
#4434=LINE('',#27526,#6144);
#4435=LINE('',#27528,#6145);
#4436=LINE('',#27530,#6146);
#4437=LINE('',#27531,#6147);
#4438=LINE('',#27533,#6148);
#4439=LINE('',#27534,#6149);
#4440=LINE('',#27536,#6150);
#4441=LINE('',#27538,#6151);
#4442=LINE('',#27540,#6152);
#4443=LINE('',#27542,#6153);
#4444=LINE('',#27544,#6154);
#4445=LINE('',#27546,#6155);
#4446=LINE('',#27548,#6156);
#4447=LINE('',#27550,#6157);
#4448=LINE('',#27551,#6158);
#4449=LINE('',#27558,#6159);
#4450=LINE('',#27560,#6160);
#4451=LINE('',#27584,#6161);
#4452=LINE('',#27660,#6162);
#4453=LINE('',#27736,#6163);
#4454=LINE('',#27814,#6164);
#4455=LINE('',#27890,#6165);
#4456=LINE('',#27966,#6166);
#4457=LINE('',#28042,#6167);
#4458=LINE('',#28118,#6168);
#4459=LINE('',#28196,#6169);
#4460=LINE('',#28272,#6170);
#4461=LINE('',#28348,#6171);
#4462=LINE('',#28426,#6172);
#4463=LINE('',#28502,#6173);
#4464=LINE('',#28578,#6174);
#4465=LINE('',#28654,#6175);
#4466=LINE('',#28732,#6176);
#4467=LINE('',#28808,#6177);
#4468=LINE('',#28884,#6178);
#4469=LINE('',#28957,#6179);
#4470=LINE('',#28962,#6180);
#4471=LINE('',#28973,#6181);
#4472=LINE('',#28983,#6182);
#4473=LINE('',#28994,#6183);
#4474=LINE('',#29024,#6184);
#4475=LINE('',#29054,#6185);
#4476=LINE('',#29084,#6186);
#4477=LINE('',#29114,#6187);
#4478=LINE('',#29144,#6188);
#4479=LINE('',#29174,#6189);
#4480=LINE('',#29204,#6190);
#4481=LINE('',#29234,#6191);
#4482=LINE('',#29264,#6192);
#4483=LINE('',#29294,#6193);
#4484=LINE('',#29324,#6194);
#4485=LINE('',#29354,#6195);
#4486=LINE('',#29384,#6196);
#4487=LINE('',#29414,#6197);
#4488=LINE('',#29444,#6198);
#4489=LINE('',#29474,#6199);
#4490=LINE('',#29504,#6200);
#4491=LINE('',#29534,#6201);
#4492=LINE('',#29544,#6202);
#4493=LINE('',#29555,#6203);
#4494=LINE('',#29622,#6204);
#4495=LINE('',#29698,#6205);
#4496=LINE('',#29774,#6206);
#4497=LINE('',#29786,#6207);
#4498=LINE('',#29799,#6208);
#4499=LINE('',#29837,#6209);
#4500=LINE('',#29875,#6210);
#4501=LINE('',#29913,#6211);
#4502=LINE('',#29951,#6212);
#4503=LINE('',#29989,#6213);
#4504=LINE('',#30027,#6214);
#4505=LINE('',#30065,#6215);
#4506=LINE('',#30112,#6216);
#4507=LINE('',#30190,#6217);
#4508=LINE('',#30266,#6218);
#4509=LINE('',#30295,#6219);
#4510=LINE('',#30400,#6220);
#4511=LINE('',#30402,#6221);
#4512=LINE('',#30403,#6222);
#4513=LINE('',#30410,#6223);
#4514=LINE('',#30411,#6224);
#4515=LINE('',#30418,#6225);
#4516=LINE('',#30419,#6226);
#4517=LINE('',#30426,#6227);
#4518=LINE('',#30427,#6228);
#4519=LINE('',#30431,#6229);
#4520=LINE('',#30433,#6230);
#4521=LINE('',#30435,#6231);
#4522=LINE('',#30444,#6232);
#4523=LINE('',#30445,#6233);
#4524=LINE('',#30446,#6234);
#4525=LINE('',#30452,#6235);
#4526=LINE('',#30459,#6236);
#4527=LINE('',#30460,#6237);
#4528=LINE('',#30464,#6238);
#4529=LINE('',#30466,#6239);
#4530=LINE('',#30468,#6240);
#4531=LINE('',#30477,#6241);
#4532=LINE('',#30478,#6242);
#4533=LINE('',#30479,#6243);
#4534=LINE('',#30485,#6244);
#4535=LINE('',#30492,#6245);
#4536=LINE('',#30493,#6246);
#4537=LINE('',#30497,#6247);
#4538=LINE('',#30499,#6248);
#4539=LINE('',#30501,#6249);
#4540=LINE('',#30512,#6250);
#4541=LINE('',#30513,#6251);
#4542=LINE('',#30514,#6252);
#4543=LINE('',#30524,#6253);
#4544=LINE('',#30531,#6254);
#4545=LINE('',#30532,#6255);
#4546=LINE('',#30541,#6256);
#4547=LINE('',#30572,#6257);
#4548=LINE('',#30581,#6258);
#4549=LINE('',#30851,#6259);
#4550=LINE('',#30862,#6260);
#4551=LINE('',#31182,#6261);
#4552=LINE('',#31193,#6262);
#4553=LINE('',#31195,#6263);
#4554=LINE('',#31203,#6264);
#4555=LINE('',#31206,#6265);
#4556=LINE('',#31224,#6266);
#4557=LINE('',#31230,#6267);
#4558=LINE('',#31248,#6268);
#4559=LINE('',#31271,#6269);
#4560=LINE('',#31277,#6270);
#4561=LINE('',#31284,#6271);
#4562=LINE('',#31291,#6272);
#4563=LINE('',#31296,#6273);
#4564=LINE('',#31301,#6274);
#4565=LINE('',#31303,#6275);
#4566=LINE('',#31305,#6276);
#4567=LINE('',#31306,#6277);
#4568=LINE('',#31309,#6278);
#4569=LINE('',#31311,#6279);
#4570=LINE('',#31312,#6280);
#4571=LINE('',#31315,#6281);
#4572=LINE('',#31317,#6282);
#4573=LINE('',#31318,#6283);
#4574=LINE('',#31321,#6284);
#4575=LINE('',#31323,#6285);
#4576=LINE('',#31324,#6286);
#4577=LINE('',#31327,#6287);
#4578=LINE('',#31329,#6288);
#4579=LINE('',#31330,#6289);
#4580=LINE('',#31333,#6290);
#4581=LINE('',#31335,#6291);
#4582=LINE('',#31336,#6292);
#4583=LINE('',#31339,#6293);
#4584=LINE('',#31341,#6294);
#4585=LINE('',#31342,#6295);
#4586=LINE('',#31345,#6296);
#4587=LINE('',#31347,#6297);
#4588=LINE('',#31348,#6298);
#4589=LINE('',#31351,#6299);
#4590=LINE('',#31353,#6300);
#4591=LINE('',#31354,#6301);
#4592=LINE('',#31357,#6302);
#4593=LINE('',#31359,#6303);
#4594=LINE('',#31360,#6304);
#4595=LINE('',#31363,#6305);
#4596=LINE('',#31365,#6306);
#4597=LINE('',#31366,#6307);
#4598=LINE('',#31369,#6308);
#4599=LINE('',#31371,#6309);
#4600=LINE('',#31372,#6310);
#4601=LINE('',#31375,#6311);
#4602=LINE('',#31377,#6312);
#4603=LINE('',#31378,#6313);
#4604=LINE('',#31381,#6314);
#4605=LINE('',#31383,#6315);
#4606=LINE('',#31384,#6316);
#4607=LINE('',#31387,#6317);
#4608=LINE('',#31389,#6318);
#4609=LINE('',#31390,#6319);
#4610=LINE('',#31393,#6320);
#4611=LINE('',#31395,#6321);
#4612=LINE('',#31396,#6322);
#4613=LINE('',#31399,#6323);
#4614=LINE('',#31401,#6324);
#4615=LINE('',#31402,#6325);
#4616=LINE('',#31405,#6326);
#4617=LINE('',#31407,#6327);
#4618=LINE('',#31408,#6328);
#4619=LINE('',#31411,#6329);
#4620=LINE('',#31413,#6330);
#4621=LINE('',#31414,#6331);
#4622=LINE('',#31417,#6332);
#4623=LINE('',#31419,#6333);
#4624=LINE('',#31420,#6334);
#4625=LINE('',#31423,#6335);
#4626=LINE('',#31425,#6336);
#4627=LINE('',#31426,#6337);
#4628=LINE('',#31429,#6338);
#4629=LINE('',#31431,#6339);
#4630=LINE('',#31432,#6340);
#4631=LINE('',#31435,#6341);
#4632=LINE('',#31437,#6342);
#4633=LINE('',#31438,#6343);
#4634=LINE('',#31441,#6344);
#4635=LINE('',#31443,#6345);
#4636=LINE('',#31444,#6346);
#4637=LINE('',#31447,#6347);
#4638=LINE('',#31449,#6348);
#4639=LINE('',#31450,#6349);
#4640=LINE('',#31453,#6350);
#4641=LINE('',#31455,#6351);
#4642=LINE('',#31456,#6352);
#4643=LINE('',#31459,#6353);
#4644=LINE('',#31461,#6354);
#4645=LINE('',#31462,#6355);
#4646=LINE('',#31465,#6356);
#4647=LINE('',#31467,#6357);
#4648=LINE('',#31468,#6358);
#4649=LINE('',#31471,#6359);
#4650=LINE('',#31473,#6360);
#4651=LINE('',#31474,#6361);
#4652=LINE('',#31477,#6362);
#4653=LINE('',#31479,#6363);
#4654=LINE('',#31480,#6364);
#4655=LINE('',#31483,#6365);
#4656=LINE('',#31485,#6366);
#4657=LINE('',#31486,#6367);
#4658=LINE('',#31489,#6368);
#4659=LINE('',#31491,#6369);
#4660=LINE('',#31492,#6370);
#4661=LINE('',#31495,#6371);
#4662=LINE('',#31497,#6372);
#4663=LINE('',#31498,#6373);
#4664=LINE('',#31501,#6374);
#4665=LINE('',#31503,#6375);
#4666=LINE('',#31504,#6376);
#4667=LINE('',#31507,#6377);
#4668=LINE('',#31509,#6378);
#4669=LINE('',#31510,#6379);
#4670=LINE('',#31513,#6380);
#4671=LINE('',#31515,#6381);
#4672=LINE('',#31516,#6382);
#4673=LINE('',#31519,#6383);
#4674=LINE('',#31521,#6384);
#4675=LINE('',#31522,#6385);
#4676=LINE('',#31525,#6386);
#4677=LINE('',#31527,#6387);
#4678=LINE('',#31528,#6388);
#4679=LINE('',#31531,#6389);
#4680=LINE('',#31533,#6390);
#4681=LINE('',#31534,#6391);
#4682=LINE('',#31537,#6392);
#4683=LINE('',#31539,#6393);
#4684=LINE('',#31540,#6394);
#4685=LINE('',#31543,#6395);
#4686=LINE('',#31545,#6396);
#4687=LINE('',#31546,#6397);
#4688=LINE('',#31549,#6398);
#4689=LINE('',#31551,#6399);
#4690=LINE('',#31552,#6400);
#4691=LINE('',#31555,#6401);
#4692=LINE('',#31557,#6402);
#4693=LINE('',#31558,#6403);
#4694=LINE('',#31561,#6404);
#4695=LINE('',#31563,#6405);
#4696=LINE('',#31564,#6406);
#4697=LINE('',#31567,#6407);
#4698=LINE('',#31569,#6408);
#4699=LINE('',#31570,#6409);
#4700=LINE('',#31573,#6410);
#4701=LINE('',#31575,#6411);
#4702=LINE('',#31576,#6412);
#4703=LINE('',#31579,#6413);
#4704=LINE('',#31581,#6414);
#4705=LINE('',#31582,#6415);
#4706=LINE('',#31585,#6416);
#4707=LINE('',#31587,#6417);
#4708=LINE('',#31588,#6418);
#4709=LINE('',#31591,#6419);
#4710=LINE('',#31593,#6420);
#4711=LINE('',#31594,#6421);
#4712=LINE('',#31597,#6422);
#4713=LINE('',#31599,#6423);
#4714=LINE('',#31600,#6424);
#4715=LINE('',#31603,#6425);
#4716=LINE('',#31605,#6426);
#4717=LINE('',#31606,#6427);
#4718=LINE('',#31609,#6428);
#4719=LINE('',#31611,#6429);
#4720=LINE('',#31612,#6430);
#4721=LINE('',#31615,#6431);
#4722=LINE('',#31617,#6432);
#4723=LINE('',#31618,#6433);
#4724=LINE('',#31621,#6434);
#4725=LINE('',#31623,#6435);
#4726=LINE('',#31624,#6436);
#4727=LINE('',#31627,#6437);
#4728=LINE('',#31629,#6438);
#4729=LINE('',#31630,#6439);
#4730=LINE('',#31633,#6440);
#4731=LINE('',#31635,#6441);
#4732=LINE('',#31636,#6442);
#4733=LINE('',#31639,#6443);
#4734=LINE('',#31641,#6444);
#4735=LINE('',#31642,#6445);
#4736=LINE('',#31645,#6446);
#4737=LINE('',#31647,#6447);
#4738=LINE('',#31648,#6448);
#4739=LINE('',#31651,#6449);
#4740=LINE('',#31653,#6450);
#4741=LINE('',#31654,#6451);
#4742=LINE('',#31657,#6452);
#4743=LINE('',#31659,#6453);
#4744=LINE('',#31660,#6454);
#4745=LINE('',#31663,#6455);
#4746=LINE('',#31665,#6456);
#4747=LINE('',#31666,#6457);
#4748=LINE('',#31669,#6458);
#4749=LINE('',#31671,#6459);
#4750=LINE('',#31672,#6460);
#4751=LINE('',#31675,#6461);
#4752=LINE('',#31677,#6462);
#4753=LINE('',#31678,#6463);
#4754=LINE('',#31681,#6464);
#4755=LINE('',#31683,#6465);
#4756=LINE('',#31684,#6466);
#4757=LINE('',#31687,#6467);
#4758=LINE('',#31689,#6468);
#4759=LINE('',#31690,#6469);
#4760=LINE('',#31693,#6470);
#4761=LINE('',#31695,#6471);
#4762=LINE('',#31696,#6472);
#4763=LINE('',#31699,#6473);
#4764=LINE('',#31701,#6474);
#4765=LINE('',#31702,#6475);
#4766=LINE('',#31705,#6476);
#4767=LINE('',#31707,#6477);
#4768=LINE('',#31708,#6478);
#4769=LINE('',#31711,#6479);
#4770=LINE('',#31713,#6480);
#4771=LINE('',#31714,#6481);
#4772=LINE('',#31717,#6482);
#4773=LINE('',#31719,#6483);
#4774=LINE('',#31720,#6484);
#4775=LINE('',#31723,#6485);
#4776=LINE('',#31725,#6486);
#4777=LINE('',#31726,#6487);
#4778=LINE('',#31729,#6488);
#4779=LINE('',#31731,#6489);
#4780=LINE('',#31732,#6490);
#4781=LINE('',#31735,#6491);
#4782=LINE('',#31737,#6492);
#4783=LINE('',#31738,#6493);
#4784=LINE('',#31741,#6494);
#4785=LINE('',#31743,#6495);
#4786=LINE('',#31744,#6496);
#4787=LINE('',#31747,#6497);
#4788=LINE('',#31749,#6498);
#4789=LINE('',#31750,#6499);
#4790=LINE('',#31753,#6500);
#4791=LINE('',#31755,#6501);
#4792=LINE('',#31756,#6502);
#4793=LINE('',#31759,#6503);
#4794=LINE('',#31761,#6504);
#4795=LINE('',#31762,#6505);
#4796=LINE('',#31765,#6506);
#4797=LINE('',#31767,#6507);
#4798=LINE('',#31768,#6508);
#4799=LINE('',#31771,#6509);
#4800=LINE('',#31773,#6510);
#4801=LINE('',#31774,#6511);
#4802=LINE('',#31777,#6512);
#4803=LINE('',#31779,#6513);
#4804=LINE('',#31780,#6514);
#4805=LINE('',#31783,#6515);
#4806=LINE('',#31785,#6516);
#4807=LINE('',#31786,#6517);
#4808=LINE('',#31789,#6518);
#4809=LINE('',#31791,#6519);
#4810=LINE('',#31792,#6520);
#4811=LINE('',#31795,#6521);
#4812=LINE('',#31797,#6522);
#4813=LINE('',#31798,#6523);
#4814=LINE('',#31801,#6524);
#4815=LINE('',#31803,#6525);
#4816=LINE('',#31804,#6526);
#4817=LINE('',#31807,#6527);
#4818=LINE('',#31809,#6528);
#4819=LINE('',#31810,#6529);
#4820=LINE('',#31813,#6530);
#4821=LINE('',#31815,#6531);
#4822=LINE('',#31816,#6532);
#4823=LINE('',#31819,#6533);
#4824=LINE('',#31821,#6534);
#4825=LINE('',#31822,#6535);
#4826=LINE('',#31825,#6536);
#4827=LINE('',#31827,#6537);
#4828=LINE('',#31828,#6538);
#4829=LINE('',#31831,#6539);
#4830=LINE('',#31833,#6540);
#4831=LINE('',#31834,#6541);
#4832=LINE('',#31836,#6542);
#4833=LINE('',#31837,#6543);
#4834=LINE('',#31852,#6544);
#4835=LINE('',#32335,#6545);
#4836=LINE('',#32383,#6546);
#4837=LINE('',#32894,#6547);
#4838=LINE('',#32895,#6548);
#4839=LINE('',#32943,#6549);
#4840=LINE('',#32950,#6550);
#4841=LINE('',#32954,#6551);
#4842=LINE('',#32958,#6552);
#4843=LINE('',#32964,#6553);
#4844=LINE('',#32967,#6554);
#4845=LINE('',#32976,#6555);
#4846=LINE('',#32981,#6556);
#4847=LINE('',#32988,#6557);
#4848=LINE('',#32993,#6558);
#4849=LINE('',#32995,#6559);
#4850=LINE('',#32997,#6560);
#4851=LINE('',#32999,#6561);
#4852=LINE('',#33001,#6562);
#4853=LINE('',#33002,#6563);
#4854=LINE('',#33006,#6564);
#4855=LINE('',#33007,#6565);
#4856=LINE('',#33008,#6566);
#4857=LINE('',#33011,#6567);
#4858=LINE('',#33012,#6568);
#4859=LINE('',#33015,#6569);
#4860=LINE('',#33016,#6570);
#4861=LINE('',#33019,#6571);
#4862=LINE('',#33020,#6572);
#4863=LINE('',#33023,#6573);
#4864=LINE('',#33024,#6574);
#4865=LINE('',#33026,#6575);
#4866=LINE('',#33086,#6576);
#4867=LINE('',#33088,#6577);
#4868=LINE('',#33090,#6578);
#4869=LINE('',#33092,#6579);
#4870=LINE('',#33094,#6580);
#4871=LINE('',#33151,#6581);
#4872=LINE('',#33211,#6582);
#4873=LINE('',#33212,#6583);
#4874=LINE('',#33259,#6584);
#4875=LINE('',#33262,#6585);
#4876=LINE('',#33263,#6586);
#4877=LINE('',#33266,#6587);
#4878=LINE('',#33267,#6588);
#4879=LINE('',#33270,#6589);
#4880=LINE('',#33271,#6590);
#4881=LINE('',#33274,#6591);
#4882=LINE('',#33275,#6592);
#4883=LINE('',#33278,#6593);
#4884=LINE('',#33279,#6594);
#4885=LINE('',#33326,#6595);
#4886=LINE('',#33385,#6596);
#4887=LINE('',#33444,#6597);
#4888=LINE('',#33447,#6598);
#4889=LINE('',#33448,#6599);
#4890=LINE('',#33509,#6600);
#4891=LINE('',#33511,#6601);
#4892=LINE('',#33513,#6602);
#4893=LINE('',#33515,#6603);
#4894=LINE('',#33516,#6604);
#4895=LINE('',#33520,#6605);
#4896=LINE('',#33521,#6606);
#4897=LINE('',#33522,#6607);
#4898=LINE('',#33526,#6608);
#4899=LINE('',#33527,#6609);
#4900=LINE('',#33528,#6610);
#4901=LINE('',#33532,#6611);
#4902=LINE('',#33534,#6612);
#4903=LINE('',#33536,#6613);
#4904=LINE('',#33537,#6614);
#4905=LINE('',#33541,#6615);
#4906=LINE('',#33542,#6616);
#4907=LINE('',#33543,#6617);
#4908=LINE('',#33547,#6618);
#4909=LINE('',#33549,#6619);
#4910=LINE('',#33550,#6620);
#4911=LINE('',#33551,#6621);
#4912=LINE('',#33555,#6622);
#4913=LINE('',#33557,#6623);
#4914=LINE('',#33559,#6624);
#4915=LINE('',#33560,#6625);
#4916=LINE('',#33564,#6626);
#4917=LINE('',#33566,#6627);
#4918=LINE('',#33568,#6628);
#4919=LINE('',#33569,#6629);
#4920=LINE('',#33570,#6630);
#4921=LINE('',#33580,#6631);
#4922=LINE('',#33584,#6632);
#4923=LINE('',#33588,#6633);
#4924=LINE('',#33590,#6634);
#4925=LINE('',#33592,#6635);
#4926=LINE('',#33594,#6636);
#4927=LINE('',#33596,#6637);
#4928=LINE('',#33597,#6638);
#4929=LINE('',#33600,#6639);
#4930=LINE('',#33602,#6640);
#4931=LINE('',#33603,#6641);
#4932=LINE('',#33607,#6642);
#4933=LINE('',#33609,#6643);
#4934=LINE('',#33610,#6644);
#4935=LINE('',#33612,#6645);
#4936=LINE('',#33613,#6646);
#4937=LINE('',#33615,#6647);
#4938=LINE('',#33616,#6648);
#4939=LINE('',#33619,#6649);
#4940=LINE('',#33620,#6650);
#4941=LINE('',#33624,#6651);
#4942=LINE('',#33626,#6652);
#4943=LINE('',#33628,#6653);
#4944=LINE('',#33629,#6654);
#4945=LINE('',#33637,#6655);
#4946=LINE('',#33639,#6656);
#4947=LINE('',#33641,#6657);
#4948=LINE('',#33642,#6658);
#4949=LINE('',#33648,#6659);
#4950=LINE('',#33649,#6660);
#4951=LINE('',#33650,#6661);
#4952=LINE('',#33652,#6662);
#4953=LINE('',#33654,#6663);
#4954=LINE('',#33656,#6664);
#4955=LINE('',#33660,#6665);
#4956=LINE('',#33662,#6666);
#4957=LINE('',#33663,#6667);
#4958=LINE('',#33665,#6668);
#4959=LINE('',#33666,#6669);
#4960=LINE('',#33668,#6670);
#4961=LINE('',#33678,#6671);
#4962=LINE('',#33682,#6672);
#4963=LINE('',#33685,#6673);
#4964=LINE('',#33687,#6674);
#4965=LINE('',#33689,#6675);
#4966=LINE('',#33691,#6676);
#4967=LINE('',#33692,#6677);
#4968=LINE('',#33695,#6678);
#4969=LINE('',#33696,#6679);
#4970=LINE('',#33700,#6680);
#4971=LINE('',#33701,#6681);
#4972=LINE('',#33703,#6682);
#4973=LINE('',#33704,#6683);
#4974=LINE('',#33706,#6684);
#4975=LINE('',#33707,#6685);
#4976=LINE('',#33711,#6686);
#4977=LINE('',#33713,#6687);
#4978=LINE('',#33714,#6688);
#4979=LINE('',#33718,#6689);
#4980=LINE('',#33720,#6690);
#4981=LINE('',#33722,#6691);
#4982=LINE('',#33724,#6692);
#4983=LINE('',#33726,#6693);
#4984=LINE('',#33727,#6694);
#4985=LINE('',#33729,#6695);
#4986=LINE('',#33730,#6696);
#4987=LINE('',#33731,#6697);
#4988=LINE('',#33733,#6698);
#4989=LINE('',#33734,#6699);
#4990=LINE('',#33735,#6700);
#4991=LINE('',#33737,#6701);
#4992=LINE('',#33738,#6702);
#4993=LINE('',#33739,#6703);
#4994=LINE('',#33741,#6704);
#4995=LINE('',#33743,#6705);
#4996=LINE('',#33745,#6706);
#4997=LINE('',#33746,#6707);
#4998=LINE('',#33749,#6708);
#4999=LINE('',#33763,#6709);
#5000=LINE('',#33765,#6710);
#5001=LINE('',#33769,#6711);
#5002=LINE('',#33771,#6712);
#5003=LINE('',#33799,#6713);
#5004=LINE('',#33875,#6714);
#5005=LINE('',#33953,#6715);
#5006=LINE('',#34029,#6716);
#5007=LINE('',#34105,#6717);
#5008=LINE('',#34181,#6718);
#5009=LINE('',#34259,#6719);
#5010=LINE('',#34335,#6720);
#5011=LINE('',#34411,#6721);
#5012=LINE('',#34489,#6722);
#5013=LINE('',#34565,#6723);
#5014=LINE('',#34641,#6724);
#5015=LINE('',#34717,#6725);
#5016=LINE('',#34731,#6726);
#5017=LINE('',#34741,#6727);
#5018=LINE('',#34752,#6728);
#5019=LINE('',#34782,#6729);
#5020=LINE('',#34812,#6730);
#5021=LINE('',#34842,#6731);
#5022=LINE('',#34872,#6732);
#5023=LINE('',#34902,#6733);
#5024=LINE('',#34932,#6734);
#5025=LINE('',#34962,#6735);
#5026=LINE('',#34992,#6736);
#5027=LINE('',#35022,#6737);
#5028=LINE('',#35052,#6738);
#5029=LINE('',#35082,#6739);
#5030=LINE('',#35112,#6740);
#5031=LINE('',#35122,#6741);
#5032=LINE('',#35134,#6742);
#5033=LINE('',#35140,#6743);
#5034=LINE('',#35146,#6744);
#5035=LINE('',#35181,#6745);
#5036=LINE('',#35183,#6746);
#5037=LINE('',#35209,#6747);
#5038=LINE('',#35548,#6748);
#5039=LINE('',#35562,#6749);
#5040=LINE('',#35951,#6750);
#5041=LINE('',#35996,#6751);
#5042=LINE('',#35998,#6752);
#5043=LINE('',#36004,#6753);
#5044=LINE('',#36007,#6754);
#5045=LINE('',#36014,#6755);
#5046=LINE('',#36032,#6756);
#5047=LINE('',#36036,#6757);
#5048=LINE('',#36042,#6758);
#5049=LINE('',#36045,#6759);
#5050=LINE('',#36050,#6760);
#5051=LINE('',#36055,#6761);
#5052=LINE('',#36057,#6762);
#5053=LINE('',#36059,#6763);
#5054=LINE('',#36061,#6764);
#5055=LINE('',#36063,#6765);
#5056=LINE('',#36065,#6766);
#5057=LINE('',#36067,#6767);
#5058=LINE('',#36071,#6768);
#5059=LINE('',#36073,#6769);
#5060=LINE('',#36075,#6770);
#5061=LINE('',#36077,#6771);
#5062=LINE('',#36079,#6772);
#5063=LINE('',#36080,#6773);
#5064=LINE('',#36086,#6774);
#5065=LINE('',#36089,#6775);
#5066=LINE('',#36093,#6776);
#5067=LINE('',#36095,#6777);
#5068=LINE('',#36097,#6778);
#5069=LINE('',#36099,#6779);
#5070=LINE('',#36101,#6780);
#5071=LINE('',#36103,#6781);
#5072=LINE('',#36105,#6782);
#5073=LINE('',#36107,#6783);
#5074=LINE('',#36109,#6784);
#5075=LINE('',#36113,#6785);
#5076=LINE('',#36115,#6786);
#5077=LINE('',#36117,#6787);
#5078=LINE('',#36118,#6788);
#5079=LINE('',#36123,#6789);
#5080=LINE('',#36125,#6790);
#5081=LINE('',#36127,#6791);
#5082=LINE('',#36129,#6792);
#5083=LINE('',#36131,#6793);
#5084=LINE('',#36132,#6794);
#5085=LINE('',#36135,#6795);
#5086=LINE('',#36139,#6796);
#5087=LINE('',#36141,#6797);
#5088=LINE('',#36145,#6798);
#5089=LINE('',#36148,#6799);
#5090=LINE('',#36150,#6800);
#5091=LINE('',#36152,#6801);
#5092=LINE('',#36154,#6802);
#5093=LINE('',#36156,#6803);
#5094=LINE('',#36158,#6804);
#5095=LINE('',#36160,#6805);
#5096=LINE('',#36162,#6806);
#5097=LINE('',#36164,#6807);
#5098=LINE('',#36169,#6808);
#5099=LINE('',#36172,#6809);
#5100=LINE('',#36174,#6810);
#5101=LINE('',#36178,#6811);
#5102=LINE('',#36183,#6812);
#5103=LINE('',#36185,#6813);
#5104=LINE('',#36189,#6814);
#5105=LINE('',#36192,#6815);
#5106=LINE('',#36194,#6816);
#5107=LINE('',#36199,#6817);
#5108=LINE('',#36202,#6818);
#5109=LINE('',#36204,#6819);
#5110=LINE('',#36208,#6820);
#5111=LINE('',#36212,#6821);
#5112=LINE('',#36214,#6822);
#5113=LINE('',#36215,#6823);
#5114=LINE('',#36217,#6824);
#5115=LINE('',#36218,#6825);
#5116=LINE('',#36220,#6826);
#5117=LINE('',#36226,#6827);
#5118=LINE('',#36228,#6828);
#5119=LINE('',#36229,#6829);
#5120=LINE('',#36231,#6830);
#5121=LINE('',#36232,#6831);
#5122=LINE('',#36234,#6832);
#5123=LINE('',#36243,#6833);
#5124=LINE('',#36245,#6834);
#5125=LINE('',#36246,#6835);
#5126=LINE('',#36249,#6836);
#5127=LINE('',#36250,#6837);
#5128=LINE('',#36253,#6838);
#5129=LINE('',#36254,#6839);
#5130=LINE('',#36257,#6840);
#5131=LINE('',#36258,#6841);
#5132=LINE('',#36261,#6842);
#5133=LINE('',#36262,#6843);
#5134=LINE('',#36264,#6844);
#5135=LINE('',#36268,#6845);
#5136=LINE('',#36270,#6846);
#5137=LINE('',#36272,#6847);
#5138=LINE('',#36274,#6848);
#5139=LINE('',#36276,#6849);
#5140=LINE('',#36277,#6850);
#5141=LINE('',#36291,#6851);
#5142=LINE('',#36297,#6852);
#5143=LINE('',#36302,#6853);
#5144=LINE('',#36304,#6854);
#5145=LINE('',#36306,#6855);
#5146=LINE('',#36307,#6856);
#5147=LINE('',#36312,#6857);
#5148=LINE('',#36316,#6858);
#5149=LINE('',#36318,#6859);
#5150=LINE('',#36319,#6860);
#5151=LINE('',#36322,#6861);
#5152=LINE('',#36324,#6862);
#5153=LINE('',#36325,#6863);
#5154=LINE('',#36328,#6864);
#5155=LINE('',#36330,#6865);
#5156=LINE('',#36331,#6866);
#5157=LINE('',#36334,#6867);
#5158=LINE('',#36336,#6868);
#5159=LINE('',#36337,#6869);
#5160=LINE('',#36340,#6870);
#5161=LINE('',#36342,#6871);
#5162=LINE('',#36343,#6872);
#5163=LINE('',#36346,#6873);
#5164=LINE('',#36348,#6874);
#5165=LINE('',#36349,#6875);
#5166=LINE('',#36352,#6876);
#5167=LINE('',#36354,#6877);
#5168=LINE('',#36355,#6878);
#5169=LINE('',#36358,#6879);
#5170=LINE('',#36360,#6880);
#5171=LINE('',#36361,#6881);
#5172=LINE('',#36364,#6882);
#5173=LINE('',#36366,#6883);
#5174=LINE('',#36367,#6884);
#5175=LINE('',#36370,#6885);
#5176=LINE('',#36372,#6886);
#5177=LINE('',#36373,#6887);
#5178=LINE('',#36376,#6888);
#5179=LINE('',#36378,#6889);
#5180=LINE('',#36379,#6890);
#5181=LINE('',#36382,#6891);
#5182=LINE('',#36384,#6892);
#5183=LINE('',#36385,#6893);
#5184=LINE('',#36388,#6894);
#5185=LINE('',#36390,#6895);
#5186=LINE('',#36391,#6896);
#5187=LINE('',#36394,#6897);
#5188=LINE('',#36396,#6898);
#5189=LINE('',#36397,#6899);
#5190=LINE('',#36400,#6900);
#5191=LINE('',#36402,#6901);
#5192=LINE('',#36403,#6902);
#5193=LINE('',#36406,#6903);
#5194=LINE('',#36408,#6904);
#5195=LINE('',#36409,#6905);
#5196=LINE('',#36412,#6906);
#5197=LINE('',#36414,#6907);
#5198=LINE('',#36415,#6908);
#5199=LINE('',#36418,#6909);
#5200=LINE('',#36420,#6910);
#5201=LINE('',#36421,#6911);
#5202=LINE('',#36424,#6912);
#5203=LINE('',#36426,#6913);
#5204=LINE('',#36427,#6914);
#5205=LINE('',#36430,#6915);
#5206=LINE('',#36432,#6916);
#5207=LINE('',#36433,#6917);
#5208=LINE('',#36436,#6918);
#5209=LINE('',#36438,#6919);
#5210=LINE('',#36439,#6920);
#5211=LINE('',#36442,#6921);
#5212=LINE('',#36444,#6922);
#5213=LINE('',#36445,#6923);
#5214=LINE('',#36448,#6924);
#5215=LINE('',#36450,#6925);
#5216=LINE('',#36451,#6926);
#5217=LINE('',#36454,#6927);
#5218=LINE('',#36456,#6928);
#5219=LINE('',#36457,#6929);
#5220=LINE('',#36460,#6930);
#5221=LINE('',#36462,#6931);
#5222=LINE('',#36463,#6932);
#5223=LINE('',#36466,#6933);
#5224=LINE('',#36468,#6934);
#5225=LINE('',#36469,#6935);
#5226=LINE('',#36472,#6936);
#5227=LINE('',#36474,#6937);
#5228=LINE('',#36475,#6938);
#5229=LINE('',#36478,#6939);
#5230=LINE('',#36480,#6940);
#5231=LINE('',#36481,#6941);
#5232=LINE('',#36484,#6942);
#5233=LINE('',#36486,#6943);
#5234=LINE('',#36487,#6944);
#5235=LINE('',#36490,#6945);
#5236=LINE('',#36492,#6946);
#5237=LINE('',#36493,#6947);
#5238=LINE('',#36496,#6948);
#5239=LINE('',#36498,#6949);
#5240=LINE('',#36499,#6950);
#5241=LINE('',#36502,#6951);
#5242=LINE('',#36504,#6952);
#5243=LINE('',#36505,#6953);
#5244=LINE('',#36508,#6954);
#5245=LINE('',#36510,#6955);
#5246=LINE('',#36511,#6956);
#5247=LINE('',#36514,#6957);
#5248=LINE('',#36516,#6958);
#5249=LINE('',#36517,#6959);
#5250=LINE('',#36520,#6960);
#5251=LINE('',#36522,#6961);
#5252=LINE('',#36523,#6962);
#5253=LINE('',#36526,#6963);
#5254=LINE('',#36528,#6964);
#5255=LINE('',#36529,#6965);
#5256=LINE('',#36532,#6966);
#5257=LINE('',#36534,#6967);
#5258=LINE('',#36535,#6968);
#5259=LINE('',#36538,#6969);
#5260=LINE('',#36540,#6970);
#5261=LINE('',#36541,#6971);
#5262=LINE('',#36547,#6972);
#5263=LINE('',#36550,#6973);
#5264=LINE('',#36552,#6974);
#5265=LINE('',#36553,#6975);
#5266=LINE('',#36555,#6976);
#5267=LINE('',#36556,#6977);
#5268=LINE('',#36565,#6978);
#5269=LINE('',#36570,#6979);
#5270=LINE('',#36572,#6980);
#5271=LINE('',#36574,#6981);
#5272=LINE('',#36575,#6982);
#5273=LINE('',#36580,#6983);
#5274=LINE('',#36584,#6984);
#5275=LINE('',#36586,#6985);
#5276=LINE('',#36587,#6986);
#5277=LINE('',#36590,#6987);
#5278=LINE('',#36592,#6988);
#5279=LINE('',#36593,#6989);
#5280=LINE('',#36596,#6990);
#5281=LINE('',#36598,#6991);
#5282=LINE('',#36599,#6992);
#5283=LINE('',#36602,#6993);
#5284=LINE('',#36604,#6994);
#5285=LINE('',#36605,#6995);
#5286=LINE('',#36611,#6996);
#5287=LINE('',#36614,#6997);
#5288=LINE('',#36616,#6998);
#5289=LINE('',#36617,#6999);
#5290=LINE('',#36620,#7000);
#5291=LINE('',#36622,#7001);
#5292=LINE('',#36623,#7002);
#5293=LINE('',#36626,#7003);
#5294=LINE('',#36628,#7004);
#5295=LINE('',#36629,#7005);
#5296=VECTOR('',#19444,1000.);
#5297=VECTOR('',#19445,1000.);
#5298=VECTOR('',#19446,1000.);
#5299=VECTOR('',#19447,1000.);
#5300=VECTOR('',#19500,1000.);
#5301=VECTOR('',#19501,1000.);
#5302=VECTOR('',#19502,1000.);
#5303=VECTOR('',#19503,1000.);
#5304=VECTOR('',#19504,1000.);
#5305=VECTOR('',#19505,1000.);
#5306=VECTOR('',#19506,1000.);
#5307=VECTOR('',#19507,1000.);
#5308=VECTOR('',#19508,1000.);
#5309=VECTOR('',#19509,1000.);
#5310=VECTOR('',#19510,1000.);
#5311=VECTOR('',#19511,1000.);
#5312=VECTOR('',#19512,1000.);
#5313=VECTOR('',#19513,1000.);
#5314=VECTOR('',#19514,1000.);
#5315=VECTOR('',#19515,1000.);
#5316=VECTOR('',#19516,1000.);
#5317=VECTOR('',#19517,1000.);
#5318=VECTOR('',#19518,1000.);
#5319=VECTOR('',#19519,1000.);
#5320=VECTOR('',#19520,1000.);
#5321=VECTOR('',#19521,1000.);
#5322=VECTOR('',#19522,1000.);
#5323=VECTOR('',#19523,1000.);
#5324=VECTOR('',#19524,1000.);
#5325=VECTOR('',#19525,1000.);
#5326=VECTOR('',#19526,1000.);
#5327=VECTOR('',#19527,1000.);
#5328=VECTOR('',#19528,1000.);
#5329=VECTOR('',#19529,1000.);
#5330=VECTOR('',#19530,1000.);
#5331=VECTOR('',#19531,1000.);
#5332=VECTOR('',#19532,1000.);
#5333=VECTOR('',#19533,1000.);
#5334=VECTOR('',#19534,1000.);
#5335=VECTOR('',#19535,1000.);
#5336=VECTOR('',#19536,1000.);
#5337=VECTOR('',#19537,1000.);
#5338=VECTOR('',#19538,1000.);
#5339=VECTOR('',#19539,1000.);
#5340=VECTOR('',#19540,1000.);
#5341=VECTOR('',#19541,1000.);
#5342=VECTOR('',#19542,1000.);
#5343=VECTOR('',#19543,1000.);
#5344=VECTOR('',#19544,1000.);
#5345=VECTOR('',#19545,1000.);
#5346=VECTOR('',#19546,1000.);
#5347=VECTOR('',#19547,1000.);
#5348=VECTOR('',#19548,1000.);
#5349=VECTOR('',#19549,1000.);
#5350=VECTOR('',#19550,1000.);
#5351=VECTOR('',#19551,1000.);
#5352=VECTOR('',#19552,1000.);
#5353=VECTOR('',#19553,1000.);
#5354=VECTOR('',#19554,1000.);
#5355=VECTOR('',#19555,1000.);
#5356=VECTOR('',#19556,1000.);
#5357=VECTOR('',#19557,1000.);
#5358=VECTOR('',#19558,1000.);
#5359=VECTOR('',#19559,1000.);
#5360=VECTOR('',#19560,1000.);
#5361=VECTOR('',#19561,1000.);
#5362=VECTOR('',#19562,1000.);
#5363=VECTOR('',#19563,1000.);
#5364=VECTOR('',#19564,1000.);
#5365=VECTOR('',#19565,1000.);
#5366=VECTOR('',#19566,1000.);
#5367=VECTOR('',#19567,1000.);
#5368=VECTOR('',#19568,1000.);
#5369=VECTOR('',#19569,1000.);
#5370=VECTOR('',#19570,1000.);
#5371=VECTOR('',#19571,1000.);
#5372=VECTOR('',#19572,1000.);
#5373=VECTOR('',#19573,1000.);
#5374=VECTOR('',#19574,1000.);
#5375=VECTOR('',#19575,1000.);
#5376=VECTOR('',#19576,1000.);
#5377=VECTOR('',#19577,1000.);
#5378=VECTOR('',#19578,1000.);
#5379=VECTOR('',#19579,1000.);
#5380=VECTOR('',#19580,1000.);
#5381=VECTOR('',#19581,1000.);
#5382=VECTOR('',#19582,1000.);
#5383=VECTOR('',#19583,1000.);
#5384=VECTOR('',#19584,1000.);
#5385=VECTOR('',#19585,1000.);
#5386=VECTOR('',#19586,1000.);
#5387=VECTOR('',#19587,1000.);
#5388=VECTOR('',#19588,1000.);
#5389=VECTOR('',#19589,1000.);
#5390=VECTOR('',#19590,1000.);
#5391=VECTOR('',#19591,1000.);
#5392=VECTOR('',#19592,1000.);
#5393=VECTOR('',#19593,1000.);
#5394=VECTOR('',#19594,1000.);
#5395=VECTOR('',#19595,1000.);
#5396=VECTOR('',#19596,1000.);
#5397=VECTOR('',#19597,1000.);
#5398=VECTOR('',#19598,1000.);
#5399=VECTOR('',#19599,1000.);
#5400=VECTOR('',#19600,1000.);
#5401=VECTOR('',#19601,1000.);
#5402=VECTOR('',#19602,1000.);
#5403=VECTOR('',#19603,1000.);
#5404=VECTOR('',#19606,1000.);
#5405=VECTOR('',#19607,1000.);
#5406=VECTOR('',#19608,1000.);
#5407=VECTOR('',#19609,1000.);
#5408=VECTOR('',#19610,1000.);
#5409=VECTOR('',#19611,1000.);
#5410=VECTOR('',#19612,1000.);
#5411=VECTOR('',#19613,1000.);
#5412=VECTOR('',#19614,1000.);
#5413=VECTOR('',#19615,1000.);
#5414=VECTOR('',#19616,1000.);
#5415=VECTOR('',#19617,1000.);
#5416=VECTOR('',#19618,1000.);
#5417=VECTOR('',#19619,1000.);
#5418=VECTOR('',#19620,1000.);
#5419=VECTOR('',#19621,1000.);
#5420=VECTOR('',#19622,1000.);
#5421=VECTOR('',#19623,1000.);
#5422=VECTOR('',#19624,1000.);
#5423=VECTOR('',#19625,1000.);
#5424=VECTOR('',#19626,1000.);
#5425=VECTOR('',#19627,1000.);
#5426=VECTOR('',#19628,1000.);
#5427=VECTOR('',#19629,1000.);
#5428=VECTOR('',#19630,1000.);
#5429=VECTOR('',#19631,1000.);
#5430=VECTOR('',#19632,1000.);
#5431=VECTOR('',#19633,1000.);
#5432=VECTOR('',#19634,1000.);
#5433=VECTOR('',#19635,1000.);
#5434=VECTOR('',#19636,1000.);
#5435=VECTOR('',#19637,1000.);
#5436=VECTOR('',#19638,1000.);
#5437=VECTOR('',#19639,1000.);
#5438=VECTOR('',#19640,1000.);
#5439=VECTOR('',#19641,1000.);
#5440=VECTOR('',#19642,1000.);
#5441=VECTOR('',#19643,1000.);
#5442=VECTOR('',#19644,1000.);
#5443=VECTOR('',#19645,1000.);
#5444=VECTOR('',#19646,1000.);
#5445=VECTOR('',#19647,1000.);
#5446=VECTOR('',#19648,1000.);
#5447=VECTOR('',#19649,1000.);
#5448=VECTOR('',#19650,1000.);
#5449=VECTOR('',#19651,1000.);
#5450=VECTOR('',#19652,1000.);
#5451=VECTOR('',#19653,1000.);
#5452=VECTOR('',#19654,1000.);
#5453=VECTOR('',#19655,1000.);
#5454=VECTOR('',#19656,1000.);
#5455=VECTOR('',#19657,1000.);
#5456=VECTOR('',#19658,1000.);
#5457=VECTOR('',#19659,1000.);
#5458=VECTOR('',#19660,1000.);
#5459=VECTOR('',#19661,1000.);
#5460=VECTOR('',#19662,1000.);
#5461=VECTOR('',#19663,1000.);
#5462=VECTOR('',#19664,1000.);
#5463=VECTOR('',#19665,1000.);
#5464=VECTOR('',#19666,1000.);
#5465=VECTOR('',#19667,1000.);
#5466=VECTOR('',#19668,1000.);
#5467=VECTOR('',#19669,1000.);
#5468=VECTOR('',#19670,1000.);
#5469=VECTOR('',#19671,1000.);
#5470=VECTOR('',#19672,1000.);
#5471=VECTOR('',#19673,1000.);
#5472=VECTOR('',#19674,1000.);
#5473=VECTOR('',#19675,1000.);
#5474=VECTOR('',#19676,1000.);
#5475=VECTOR('',#19677,1000.);
#5476=VECTOR('',#19678,1000.);
#5477=VECTOR('',#19679,1000.);
#5478=VECTOR('',#19680,1000.);
#5479=VECTOR('',#19681,1000.);
#5480=VECTOR('',#19682,1000.);
#5481=VECTOR('',#19683,1000.);
#5482=VECTOR('',#19684,1000.);
#5483=VECTOR('',#19685,1000.);
#5484=VECTOR('',#19686,1000.);
#5485=VECTOR('',#19687,1000.);
#5486=VECTOR('',#19688,1000.);
#5487=VECTOR('',#19689,1000.);
#5488=VECTOR('',#19690,1000.);
#5489=VECTOR('',#19691,1000.);
#5490=VECTOR('',#19692,1000.);
#5491=VECTOR('',#19693,1000.);
#5492=VECTOR('',#19694,1000.);
#5493=VECTOR('',#19695,1000.);
#5494=VECTOR('',#19696,1000.);
#5495=VECTOR('',#19697,1000.);
#5496=VECTOR('',#19698,1000.);
#5497=VECTOR('',#19699,1000.);
#5498=VECTOR('',#19700,1000.);
#5499=VECTOR('',#19701,1000.);
#5500=VECTOR('',#19702,1000.);
#5501=VECTOR('',#19703,1000.);
#5502=VECTOR('',#19704,1000.);
#5503=VECTOR('',#19705,1000.);
#5504=VECTOR('',#19706,1000.);
#5505=VECTOR('',#19707,1000.);
#5506=VECTOR('',#19708,1000.);
#5507=VECTOR('',#19709,1000.);
#5508=VECTOR('',#19710,1000.);
#5509=VECTOR('',#19711,1000.);
#5510=VECTOR('',#19712,1000.);
#5511=VECTOR('',#19713,1000.);
#5512=VECTOR('',#19768,1000.);
#5513=VECTOR('',#19769,1000.);
#5514=VECTOR('',#19772,0.750000000000001);
#5515=VECTOR('',#19775,0.750000000000001);
#5516=VECTOR('',#19778,0.75);
#5517=VECTOR('',#19781,0.75);
#5518=VECTOR('',#19784,0.75);
#5519=VECTOR('',#19787,0.75);
#5520=VECTOR('',#19790,0.750000000000001);
#5521=VECTOR('',#19793,0.750000000000001);
#5522=VECTOR('',#19796,0.750000000000001);
#5523=VECTOR('',#19799,0.750000000000001);
#5524=VECTOR('',#19802,0.750000000000001);
#5525=VECTOR('',#19805,0.750000000000001);
#5526=VECTOR('',#19808,0.750000000000001);
#5527=VECTOR('',#19811,0.750000000000001);
#5528=VECTOR('',#19814,0.750000000000001);
#5529=VECTOR('',#19817,0.750000000000001);
#5530=VECTOR('',#19820,0.750000000000001);
#5531=VECTOR('',#19823,0.750000000000001);
#5532=VECTOR('',#19826,0.750000000000001);
#5533=VECTOR('',#19829,0.750000000000001);
#5534=VECTOR('',#19832,0.750000000000001);
#5535=VECTOR('',#19835,0.750000000000001);
#5536=VECTOR('',#19838,0.750000000000001);
#5537=VECTOR('',#19841,0.750000000000001);
#5538=VECTOR('',#19844,0.750000000000001);
#5539=VECTOR('',#19847,0.750000000000001);
#5540=VECTOR('',#19850,1000.);
#5541=VECTOR('',#19851,1000.);
#5542=VECTOR('',#19854,1000.);
#5543=VECTOR('',#19855,1000.);
#5544=VECTOR('',#19858,1000.);
#5545=VECTOR('',#19859,1000.);
#5546=VECTOR('',#19862,1000.);
#5547=VECTOR('',#19863,1000.);
#5548=VECTOR('',#19866,1000.);
#5549=VECTOR('',#19867,1000.);
#5550=VECTOR('',#19870,1000.);
#5551=VECTOR('',#19871,1000.);
#5552=VECTOR('',#19874,1000.);
#5553=VECTOR('',#19875,1000.);
#5554=VECTOR('',#19878,1000.);
#5555=VECTOR('',#19879,1000.);
#5556=VECTOR('',#19882,1000.);
#5557=VECTOR('',#19883,1000.);
#5558=VECTOR('',#19886,1000.);
#5559=VECTOR('',#19887,1000.);
#5560=VECTOR('',#19890,1000.);
#5561=VECTOR('',#19891,1000.);
#5562=VECTOR('',#19894,1000.);
#5563=VECTOR('',#19895,1000.);
#5564=VECTOR('',#19898,1000.);
#5565=VECTOR('',#19899,1000.);
#5566=VECTOR('',#19902,1000.);
#5567=VECTOR('',#19903,1000.);
#5568=VECTOR('',#19906,1000.);
#5569=VECTOR('',#19907,1000.);
#5570=VECTOR('',#19910,1000.);
#5571=VECTOR('',#19911,1000.);
#5572=VECTOR('',#19914,1000.);
#5573=VECTOR('',#19915,1000.);
#5574=VECTOR('',#19918,1000.);
#5575=VECTOR('',#19919,1000.);
#5576=VECTOR('',#19922,1000.);
#5577=VECTOR('',#19923,1000.);
#5578=VECTOR('',#19926,1000.);
#5579=VECTOR('',#19927,1000.);
#5580=VECTOR('',#19930,1000.);
#5581=VECTOR('',#19931,1000.);
#5582=VECTOR('',#19934,1000.);
#5583=VECTOR('',#19935,1000.);
#5584=VECTOR('',#19938,1000.);
#5585=VECTOR('',#19939,1000.);
#5586=VECTOR('',#19942,1000.);
#5587=VECTOR('',#19943,1000.);
#5588=VECTOR('',#19946,1000.);
#5589=VECTOR('',#19947,1000.);
#5590=VECTOR('',#19950,1000.);
#5591=VECTOR('',#19951,1000.);
#5592=VECTOR('',#19954,1000.);
#5593=VECTOR('',#19957,1000.);
#5594=VECTOR('',#19960,1000.);
#5595=VECTOR('',#19963,1000.);
#5596=VECTOR('',#19968,1000.);
#5597=VECTOR('',#19971,1000.);
#5598=VECTOR('',#19976,1000.);
#5599=VECTOR('',#19979,1000.);
#5600=VECTOR('',#19984,1000.);
#5601=VECTOR('',#19987,1000.);
#5602=VECTOR('',#19992,1000.);
#5603=VECTOR('',#19995,1000.);
#5604=VECTOR('',#20000,1000.);
#5605=VECTOR('',#20003,1000.);
#5606=VECTOR('',#20008,1000.);
#5607=VECTOR('',#20011,1000.);
#5608=VECTOR('',#20016,1000.);
#5609=VECTOR('',#20019,1000.);
#5610=VECTOR('',#20024,1000.);
#5611=VECTOR('',#20027,1000.);
#5612=VECTOR('',#20032,1000.);
#5613=VECTOR('',#20035,1000.);
#5614=VECTOR('',#20040,1000.);
#5615=VECTOR('',#20043,1000.);
#5616=VECTOR('',#20048,1000.);
#5617=VECTOR('',#20051,1000.);
#5618=VECTOR('',#20056,1000.);
#5619=VECTOR('',#20059,1000.);
#5620=VECTOR('',#20064,1000.);
#5621=VECTOR('',#20067,1000.);
#5622=VECTOR('',#20072,1000.);
#5623=VECTOR('',#20075,1000.);
#5624=VECTOR('',#20080,1000.);
#5625=VECTOR('',#20083,1000.);
#5626=VECTOR('',#20088,1000.);
#5627=VECTOR('',#20091,1000.);
#5628=VECTOR('',#20096,1000.);
#5629=VECTOR('',#20099,1000.);
#5630=VECTOR('',#20104,1000.);
#5631=VECTOR('',#20107,1000.);
#5632=VECTOR('',#20112,1000.);
#5633=VECTOR('',#20115,1000.);
#5634=VECTOR('',#20120,1000.);
#5635=VECTOR('',#20123,1000.);
#5636=VECTOR('',#20128,1000.);
#5637=VECTOR('',#20131,1000.);
#5638=VECTOR('',#20136,1000.);
#5639=VECTOR('',#20139,1000.);
#5640=VECTOR('',#20144,1000.);
#5641=VECTOR('',#20147,1000.);
#5642=VECTOR('',#20152,1000.);
#5643=VECTOR('',#20155,1000.);
#5644=VECTOR('',#20160,1000.);
#5645=VECTOR('',#20163,1000.);
#5646=VECTOR('',#20176,1000.);
#5647=VECTOR('',#20181,1000.);
#5648=VECTOR('',#20184,1000.);
#5649=VECTOR('',#20187,1000.);
#5650=VECTOR('',#20194,1000.);
#5651=VECTOR('',#20199,1000.);
#5652=VECTOR('',#20202,1000.);
#5653=VECTOR('',#20205,1000.);
#5654=VECTOR('',#20212,1000.);
#5655=VECTOR('',#20217,1000.);
#5656=VECTOR('',#20220,1000.);
#5657=VECTOR('',#20223,1000.);
#5658=VECTOR('',#20236,1000.);
#5659=VECTOR('',#20239,1000.);
#5660=VECTOR('',#20248,1000.);
#5661=VECTOR('',#20249,1000.);
#5662=VECTOR('',#20250,1000.);
#5663=VECTOR('',#20251,1000.);
#5664=VECTOR('',#20252,1000.);
#5665=VECTOR('',#20253,1000.);
#5666=VECTOR('',#20264,1000.);
#5667=VECTOR('',#20265,1000.);
#5668=VECTOR('',#20276,1000.);
#5669=VECTOR('',#20277,1000.);
#5670=VECTOR('',#20282,1000.);
#5671=VECTOR('',#20285,1000.);
#5672=VECTOR('',#20286,1000.);
#5673=VECTOR('',#20287,1000.);
#5674=VECTOR('',#20290,1000.);
#5675=VECTOR('',#20291,1000.);
#5676=VECTOR('',#20292,1000.);
#5677=VECTOR('',#20295,1000.);
#5678=VECTOR('',#20296,1000.);
#5679=VECTOR('',#20297,1000.);
#5680=VECTOR('',#20300,1000.);
#5681=VECTOR('',#20301,1000.);
#5682=VECTOR('',#20302,1000.);
#5683=VECTOR('',#20305,1000.);
#5684=VECTOR('',#20306,1000.);
#5685=VECTOR('',#20307,1000.);
#5686=VECTOR('',#20312,1000.);
#5687=VECTOR('',#20313,1000.);
#5688=VECTOR('',#20318,1000.);
#5689=VECTOR('',#20321,1000.);
#5690=VECTOR('',#20324,1000.);
#5691=VECTOR('',#20325,1000.);
#5692=VECTOR('',#20328,1000.);
#5693=VECTOR('',#20333,1000.);
#5694=VECTOR('',#20334,1000.);
#5695=VECTOR('',#20335,1000.);
#5696=VECTOR('',#20336,1000.);
#5697=VECTOR('',#20337,1000.);
#5698=VECTOR('',#20340,1000.);
#5699=VECTOR('',#20343,1000.);
#5700=VECTOR('',#20344,1000.);
#5701=VECTOR('',#20345,1000.);
#5702=VECTOR('',#20346,1000.);
#5703=VECTOR('',#20353,1000.);
#5704=VECTOR('',#20356,1000.);
#5705=VECTOR('',#20361,1000.);
#5706=VECTOR('',#20364,1000.);
#5707=VECTOR('',#20369,1000.);
#5708=VECTOR('',#20372,1000.);
#5709=VECTOR('',#20377,1000.);
#5710=VECTOR('',#20380,1000.);
#5711=VECTOR('',#20383,1000.);
#5712=VECTOR('',#20384,1000.);
#5713=VECTOR('',#20385,1000.);
#5714=VECTOR('',#20386,1000.);
#5715=VECTOR('',#20389,1000.);
#5716=VECTOR('',#20390,1000.);
#5717=VECTOR('',#20391,1000.);
#5718=VECTOR('',#20394,1000.);
#5719=VECTOR('',#20395,1000.);
#5720=VECTOR('',#20396,1000.);
#5721=VECTOR('',#20399,1000.);
#5722=VECTOR('',#20400,1000.);
#5723=VECTOR('',#20401,1000.);
#5724=VECTOR('',#20404,1000.);
#5725=VECTOR('',#20405,1000.);
#5726=VECTOR('',#20406,1000.);
#5727=VECTOR('',#20409,1000.);
#5728=VECTOR('',#20410,1000.);
#5729=VECTOR('',#20411,1000.);
#5730=VECTOR('',#20414,1000.);
#5731=VECTOR('',#20415,1000.);
#5732=VECTOR('',#20416,1000.);
#5733=VECTOR('',#20419,1000.);
#5734=VECTOR('',#20420,1000.);
#5735=VECTOR('',#20421,1000.);
#5736=VECTOR('',#20422,1000.);
#5737=VECTOR('',#20425,1000.);
#5738=VECTOR('',#20426,1000.);
#5739=VECTOR('',#20427,1000.);
#5740=VECTOR('',#20428,1000.);
#5741=VECTOR('',#20431,1000.);
#5742=VECTOR('',#20432,1000.);
#5743=VECTOR('',#20433,1000.);
#5744=VECTOR('',#20436,1000.);
#5745=VECTOR('',#20437,1000.);
#5746=VECTOR('',#20438,1000.);
#5747=VECTOR('',#20441,1000.);
#5748=VECTOR('',#20442,1000.);
#5749=VECTOR('',#20445,1000.);
#5750=VECTOR('',#20446,1000.);
#5751=VECTOR('',#20449,1000.);
#5752=VECTOR('',#20450,1000.);
#5753=VECTOR('',#20451,1000.);
#5754=VECTOR('',#20454,1000.);
#5755=VECTOR('',#20455,1000.);
#5756=VECTOR('',#20456,1000.);
#5757=VECTOR('',#20459,1000.);
#5758=VECTOR('',#20462,1000.);
#5759=VECTOR('',#20463,1000.);
#5760=VECTOR('',#20466,1000.);
#5761=VECTOR('',#20467,1000.);
#5762=VECTOR('',#20468,1000.);
#5763=VECTOR('',#20473,1000.);
#5764=VECTOR('',#20476,1000.);
#5765=VECTOR('',#20481,1000.);
#5766=VECTOR('',#20484,1000.);
#5767=VECTOR('',#20489,1000.);
#5768=VECTOR('',#20492,1000.);
#5769=VECTOR('',#20497,1000.);
#5770=VECTOR('',#20500,1000.);
#5771=VECTOR('',#20503,1000.);
#5772=VECTOR('',#20504,1000.);
#5773=VECTOR('',#20505,1000.);
#5774=VECTOR('',#20506,1000.);
#5775=VECTOR('',#20509,1000.);
#5776=VECTOR('',#20510,1000.);
#5777=VECTOR('',#20515,1000.);
#5778=VECTOR('',#20516,1000.);
#5779=VECTOR('',#20519,1000.);
#5780=VECTOR('',#20524,1000.);
#5781=VECTOR('',#20525,1000.);
#5782=VECTOR('',#20528,1000.);
#5783=VECTOR('',#20529,1000.);
#5784=VECTOR('',#20532,1000.);
#5785=VECTOR('',#20533,1000.);
#5786=VECTOR('',#20534,1000.);
#5787=VECTOR('',#20535,1000.);
#5788=VECTOR('',#20540,1000.);
#5789=VECTOR('',#20541,1000.);
#5790=VECTOR('',#20548,1000.);
#5791=VECTOR('',#20549,1000.);
#5792=VECTOR('',#20554,1000.);
#5793=VECTOR('',#20555,1000.);
#5794=VECTOR('',#20556,1000.);
#5795=VECTOR('',#20557,1000.);
#5796=VECTOR('',#20562,1000.);
#5797=VECTOR('',#20563,1000.);
#5798=VECTOR('',#20568,1000.);
#5799=VECTOR('',#20569,1000.);
#5800=VECTOR('',#20576,1000.);
#5801=VECTOR('',#20579,1000.);
#5802=VECTOR('',#20584,1000.);
#5803=VECTOR('',#20585,1000.);
#5804=VECTOR('',#20586,1000.);
#5805=VECTOR('',#20589,1000.);
#5806=VECTOR('',#20596,1000.);
#5807=VECTOR('',#20597,1000.);
#5808=VECTOR('',#20600,1000.);
#5809=VECTOR('',#20603,1000.);
#5810=VECTOR('',#20608,1000.);
#5811=VECTOR('',#20609,1000.);
#5812=VECTOR('',#20610,1000.);
#5813=VECTOR('',#20613,1000.);
#5814=VECTOR('',#20620,1000.);
#5815=VECTOR('',#20621,1000.);
#5816=VECTOR('',#20626,1000.);
#5817=VECTOR('',#20627,1000.);
#5818=VECTOR('',#20628,1000.);
#5819=VECTOR('',#20629,1000.);
#5820=VECTOR('',#20632,1000.);
#5821=VECTOR('',#20633,1000.);
#5822=VECTOR('',#20634,1000.);
#5823=VECTOR('',#20637,1000.);
#5824=VECTOR('',#20642,1000.);
#5825=VECTOR('',#20643,1000.);
#5826=VECTOR('',#20644,1000.);
#5827=VECTOR('',#20647,1000.);
#5828=VECTOR('',#20648,1000.);
#5829=VECTOR('',#20653,1000.);
#5830=VECTOR('',#20654,1000.);
#5831=VECTOR('',#20655,1000.);
#5832=VECTOR('',#20656,1000.);
#5833=VECTOR('',#20659,1000.);
#5834=VECTOR('',#20660,1000.);
#5835=VECTOR('',#20663,1000.);
#5836=VECTOR('',#20664,1000.);
#5837=VECTOR('',#20665,1000.);
#5838=VECTOR('',#20666,1000.);
#5839=VECTOR('',#20667,1000.);
#5840=VECTOR('',#20668,1000.);
#5841=VECTOR('',#20669,1000.);
#5842=VECTOR('',#20672,1000.);
#5843=VECTOR('',#20675,1000.);
#5844=VECTOR('',#20676,1000.);
#5845=VECTOR('',#20677,1000.);
#5846=VECTOR('',#20678,1000.);
#5847=VECTOR('',#20681,1000.);
#5848=VECTOR('',#20862,31.5);
#5849=VECTOR('',#20865,17.9);
#5850=VECTOR('',#20898,17.5);
#5851=VECTOR('',#20909,15.8);
#5852=VECTOR('',#20914,10.2);
#5853=VECTOR('',#20921,12.5);
#5854=VECTOR('',#20924,31.5);
#5855=VECTOR('',#20957,1000.);
#5856=VECTOR('',#20960,1000.);
#5857=VECTOR('',#20975,10.);
#5858=VECTOR('',#20976,10.);
#5859=VECTOR('',#20977,10.);
#5860=VECTOR('',#20980,1000.);
#5861=VECTOR('',#20981,1000.);
#5862=VECTOR('',#21010,1000.);
#5863=VECTOR('',#21011,1000.);
#5864=VECTOR('',#21014,10.);
#5865=VECTOR('',#21015,10.);
#5866=VECTOR('',#21016,10.);
#5867=VECTOR('',#21019,10.);
#5868=VECTOR('',#21020,10.);
#5869=VECTOR('',#21021,10.);
#5870=VECTOR('',#21026,1000.);
#5871=VECTOR('',#21029,1000.);
#5872=VECTOR('',#21034,1000.);
#5873=VECTOR('',#21035,1000.);
#5874=VECTOR('',#21056,10.);
#5875=VECTOR('',#21057,10.);
#5876=VECTOR('',#21058,10.);
#5877=VECTOR('',#21067,1000.);
#5878=VECTOR('',#21068,1000.);
#5879=VECTOR('',#21079,1000.);
#5880=VECTOR('',#21082,1000.);
#5881=VECTOR('',#21097,1000.);
#5882=VECTOR('',#21098,1000.);
#5883=VECTOR('',#21105,10.);
#5884=VECTOR('',#21106,10.);
#5885=VECTOR('',#21107,10.);
#5886=VECTOR('',#21110,1000.);
#5887=VECTOR('',#21111,1000.);
#5888=VECTOR('',#21114,1000.);
#5889=VECTOR('',#21115,1000.);
#5890=VECTOR('',#21146,1000.);
#5891=VECTOR('',#21147,1000.);
#5892=VECTOR('',#21150,10.);
#5893=VECTOR('',#21151,10.);
#5894=VECTOR('',#21152,10.);
#5895=VECTOR('',#21155,10.);
#5896=VECTOR('',#21158,10.);
#5897=VECTOR('',#21159,10.);
#5898=VECTOR('',#21162,1000.);
#5899=VECTOR('',#21165,1000.);
#5900=VECTOR('',#21170,1000.);
#5901=VECTOR('',#21171,1000.);
#5902=VECTOR('',#21194,10.);
#5903=VECTOR('',#21195,10.);
#5904=VECTOR('',#21196,10.);
#5905=VECTOR('',#21203,1000.);
#5906=VECTOR('',#21204,1000.);
#5907=VECTOR('',#21215,1000.);
#5908=VECTOR('',#21218,1000.);
#5909=VECTOR('',#21233,1000.);
#5910=VECTOR('',#21234,1000.);
#5911=VECTOR('',#21243,10.);
#5912=VECTOR('',#21244,10.);
#5913=VECTOR('',#21245,10.);
#5914=VECTOR('',#21248,1000.);
#5915=VECTOR('',#21249,1000.);
#5916=VECTOR('',#21252,1000.);
#5917=VECTOR('',#21253,1000.);
#5918=VECTOR('',#21284,1000.);
#5919=VECTOR('',#21285,1000.);
#5920=VECTOR('',#21288,10.);
#5921=VECTOR('',#21289,10.);
#5922=VECTOR('',#21290,10.);
#5923=VECTOR('',#21295,1000.);
#5924=VECTOR('',#21296,1000.);
#5925=VECTOR('',#21307,1000.);
#5926=VECTOR('',#21308,1000.);
#5927=VECTOR('',#21315,1000.);
#5928=VECTOR('',#21316,1000.);
#5929=VECTOR('',#21323,1000.);
#5930=VECTOR('',#21324,1000.);
#5931=VECTOR('',#21331,1000.);
#5932=VECTOR('',#21332,1000.);
#5933=VECTOR('',#21339,1000.);
#5934=VECTOR('',#21340,1000.);
#5935=VECTOR('',#21357,17.5);
#5936=VECTOR('',#21360,17.5);
#5937=VECTOR('',#21365,19.5);
#5938=VECTOR('',#21370,31.5);
#5939=VECTOR('',#21385,1000.);
#5940=VECTOR('',#21388,1000.);
#5941=VECTOR('',#21393,1000.);
#5942=VECTOR('',#21396,1000.);
#5943=VECTOR('',#21401,1000.);
#5944=VECTOR('',#21404,1000.);
#5945=VECTOR('',#21409,1000.);
#5946=VECTOR('',#21412,1000.);
#5947=VECTOR('',#21417,1000.);
#5948=VECTOR('',#21420,1000.);
#5949=VECTOR('',#21425,1000.);
#5950=VECTOR('',#21428,1000.);
#5951=VECTOR('',#21435,1.6);
#5952=VECTOR('',#21444,1.6);
#5953=VECTOR('',#21453,1.6);
#5954=VECTOR('',#21462,1.6);
#5955=VECTOR('',#21471,1.6);
#5956=VECTOR('',#21480,1.6);
#5957=VECTOR('',#21489,1.6);
#5958=VECTOR('',#21498,1.6);
#5959=VECTOR('',#21507,1.6);
#5960=VECTOR('',#21516,2.1);
#5961=VECTOR('',#21525,1.6);
#5962=VECTOR('',#21534,1.6);
#5963=VECTOR('',#21543,1.6);
#5964=VECTOR('',#21548,1000.);
#5965=VECTOR('',#21549,1000.);
#5966=VECTOR('',#21550,1000.);
#5967=VECTOR('',#21551,1000.);
#5968=VECTOR('',#21556,1000.);
#5969=VECTOR('',#21557,1000.);
#5970=VECTOR('',#21560,1000.);
#5971=VECTOR('',#21563,1000.);
#5972=VECTOR('',#21564,1000.);
#5973=VECTOR('',#21565,1000.);
#5974=VECTOR('',#21568,1000.);
#5975=VECTOR('',#21569,1000.);
#5976=VECTOR('',#21570,1000.);
#5977=VECTOR('',#21571,1000.);
#5978=VECTOR('',#21574,1000.);
#5979=VECTOR('',#21575,1000.);
#5980=VECTOR('',#21576,1000.);
#5981=VECTOR('',#21577,1000.);
#5982=VECTOR('',#21580,1000.);
#5983=VECTOR('',#21581,1000.);
#5984=VECTOR('',#21584,1000.);
#5985=VECTOR('',#21585,1000.);
#5986=VECTOR('',#21586,1000.);
#5987=VECTOR('',#21589,1000.);
#5988=VECTOR('',#21590,1000.);
#5989=VECTOR('',#21595,1000.);
#5990=VECTOR('',#21596,1000.);
#5991=VECTOR('',#21599,1000.);
#5992=VECTOR('',#21604,1000.);
#5993=VECTOR('',#21607,1000.);
#5994=VECTOR('',#21610,1000.);
#5995=VECTOR('',#21611,1000.);
#5996=VECTOR('',#21614,1000.);
#5997=VECTOR('',#21617,1000.);
#5998=VECTOR('',#21618,1000.);
#5999=VECTOR('',#21619,1000.);
#6000=VECTOR('',#21620,1000.);
#6001=VECTOR('',#21621,1000.);
#6002=VECTOR('',#21622,1000.);
#6003=VECTOR('',#21625,1000.);
#6004=VECTOR('',#21628,1000.);
#6005=VECTOR('',#21633,1000.);
#6006=VECTOR('',#21634,1000.);
#6007=VECTOR('',#21637,1000.);
#6008=VECTOR('',#21638,1000.);
#6009=VECTOR('',#21641,1000.);
#6010=VECTOR('',#21642,1000.);
#6011=VECTOR('',#21645,1000.);
#6012=VECTOR('',#21646,1000.);
#6013=VECTOR('',#21649,1.6);
#6014=VECTOR('',#21656,1.15469920262284);
#6015=VECTOR('',#21661,1.6);
#6016=VECTOR('',#21666,1.6);
#6017=VECTOR('',#21671,1.6);
#6018=VECTOR('',#21678,1.33321558059984);
#6019=VECTOR('',#21685,1.32106757713908);
#6020=VECTOR('',#21690,2.1);
#6021=VECTOR('',#21695,1.6);
#6022=VECTOR('',#21700,1.6);
#6023=VECTOR('',#21705,1.6);
#6024=VECTOR('',#21710,1.6);
#6025=VECTOR('',#21715,1.6);
#6026=VECTOR('',#21720,1.6);
#6027=VECTOR('',#21725,1.6);
#6028=VECTOR('',#21730,1.6);
#6029=VECTOR('',#21735,1000.);
#6030=VECTOR('',#21736,1000.);
#6031=VECTOR('',#21737,1000.);
#6032=VECTOR('',#21738,1000.);
#6033=VECTOR('',#21741,1000.);
#6034=VECTOR('',#21742,1000.);
#6035=VECTOR('',#21743,1000.);
#6036=VECTOR('',#21746,1000.);
#6037=VECTOR('',#21747,1000.);
#6038=VECTOR('',#21750,1000.);
#6039=VECTOR('',#21751,1000.);
#6040=VECTOR('',#21752,1000.);
#6041=VECTOR('',#21759,1000.);
#6042=VECTOR('',#21762,1000.);
#6043=VECTOR('',#21763,1000.);
#6044=VECTOR('',#21766,1000.);
#6045=VECTOR('',#21767,1000.);
#6046=VECTOR('',#21768,1000.);
#6047=VECTOR('',#21775,1000.);
#6048=VECTOR('',#21778,1000.);
#6049=VECTOR('',#21779,1000.);
#6050=VECTOR('',#21780,1000.);
#6051=VECTOR('',#21787,1000.);
#6052=VECTOR('',#21790,1000.);
#6053=VECTOR('',#21791,1000.);
#6054=VECTOR('',#21792,1000.);
#6055=VECTOR('',#21795,1000.);
#6056=VECTOR('',#21796,1000.);
#6057=VECTOR('',#21797,1000.);
#6058=VECTOR('',#21798,1000.);
#6059=VECTOR('',#21799,1000.);
#6060=VECTOR('',#21800,1000.);
#6061=VECTOR('',#21803,1000.);
#6062=VECTOR('',#21804,1000.);
#6063=VECTOR('',#21807,1000.);
#6064=VECTOR('',#21808,1000.);
#6065=VECTOR('',#21809,1000.);
#6066=VECTOR('',#21810,1000.);
#6067=VECTOR('',#21811,1000.);
#6068=VECTOR('',#21812,1000.);
#6069=VECTOR('',#21815,1000.);
#6070=VECTOR('',#21816,1000.);
#6071=VECTOR('',#21817,1000.);
#6072=VECTOR('',#21820,1000.);
#6073=VECTOR('',#21821,1000.);
#6074=VECTOR('',#21822,1000.);
#6075=VECTOR('',#21825,1000.);
#6076=VECTOR('',#21826,1000.);
#6077=VECTOR('',#21829,1000.);
#6078=VECTOR('',#21832,1000.);
#6079=VECTOR('',#21833,1000.);
#6080=VECTOR('',#21840,1000.);
#6081=VECTOR('',#21843,1000.);
#6082=VECTOR('',#21852,1000.);
#6083=VECTOR('',#21855,1000.);
#6084=VECTOR('',#21860,1000.);
#6085=VECTOR('',#21863,1000.);
#6086=VECTOR('',#21866,1000.);
#6087=VECTOR('',#21867,1000.);
#6088=VECTOR('',#21868,1000.);
#6089=VECTOR('',#21891,2.);
#6090=VECTOR('',#21898,2.);
#6091=VECTOR('',#21901,1000.);
#6092=VECTOR('',#21904,1000.);
#6093=VECTOR('',#21905,1000.);
#6094=VECTOR('',#21906,1000.);
#6095=VECTOR('',#21907,1000.);
#6096=VECTOR('',#21910,1000.);
#6097=VECTOR('',#21911,1000.);
#6098=VECTOR('',#21912,1000.);
#6099=VECTOR('',#21915,1000.);
#6100=VECTOR('',#21916,1000.);
#6101=VECTOR('',#21919,1000.);
#6102=VECTOR('',#21920,1000.);
#6103=VECTOR('',#21923,1000.);
#6104=VECTOR('',#21930,1000.);
#6105=VECTOR('',#21931,1000.);
#6106=VECTOR('',#21932,1000.);
#6107=VECTOR('',#21933,1000.);
#6108=VECTOR('',#21936,1000.);
#6109=VECTOR('',#21937,1000.);
#6110=VECTOR('',#21938,1000.);
#6111=VECTOR('',#21939,1000.);
#6112=VECTOR('',#21944,1000.);
#6113=VECTOR('',#21947,1000.);
#6114=VECTOR('',#21952,1000.);
#6115=VECTOR('',#21955,1000.);
#6116=VECTOR('',#21960,1000.);
#6117=VECTOR('',#21963,1000.);
#6118=VECTOR('',#21968,1000.);
#6119=VECTOR('',#21971,1000.);
#6120=VECTOR('',#21974,1000.);
#6121=VECTOR('',#21975,1000.);
#6122=VECTOR('',#21976,1000.);
#6123=VECTOR('',#21979,1000.);
#6124=VECTOR('',#21980,1000.);
#6125=VECTOR('',#21983,1000.);
#6126=VECTOR('',#21984,1000.);
#6127=VECTOR('',#21985,1000.);
#6128=VECTOR('',#21988,1000.);
#6129=VECTOR('',#21989,1000.);
#6130=VECTOR('',#21992,1000.);
#6131=VECTOR('',#21993,1000.);
#6132=VECTOR('',#21994,1000.);
#6133=VECTOR('',#21995,1000.);
#6134=VECTOR('',#21996,1000.);
#6135=VECTOR('',#21997,1000.);
#6136=VECTOR('',#21998,1000.);
#6137=VECTOR('',#21999,1000.);
#6138=VECTOR('',#22000,1000.);
#6139=VECTOR('',#22003,1000.);
#6140=VECTOR('',#22004,1000.);
#6141=VECTOR('',#22005,1000.);
#6142=VECTOR('',#22006,1000.);
#6143=VECTOR('',#22007,1000.);
#6144=VECTOR('',#22008,1000.);
#6145=VECTOR('',#22009,1000.);
#6146=VECTOR('',#22010,1000.);
#6147=VECTOR('',#22011,1000.);
#6148=VECTOR('',#22014,1000.);
#6149=VECTOR('',#22015,1000.);
#6150=VECTOR('',#22018,1000.);
#6151=VECTOR('',#22021,1000.);
#6152=VECTOR('',#22024,1000.);
#6153=VECTOR('',#22027,1000.);
#6154=VECTOR('',#22030,1000.);
#6155=VECTOR('',#22033,1000.);
#6156=VECTOR('',#22036,1000.);
#6157=VECTOR('',#22039,1000.);
#6158=VECTOR('',#22040,1000.);
#6159=VECTOR('',#22049,1.60000000000001);
#6160=VECTOR('',#22050,1000.);
#6161=VECTOR('',#22055,1.60000000000001);
#6162=VECTOR('',#22058,1.60000000000001);
#6163=VECTOR('',#22061,1.60000000000001);
#6164=VECTOR('',#22064,1.60000000000001);
#6165=VECTOR('',#22067,1.60000000000001);
#6166=VECTOR('',#22070,1.60000000000001);
#6167=VECTOR('',#22073,1.60000000000001);
#6168=VECTOR('',#22076,1.60000000000001);
#6169=VECTOR('',#22079,1.60000000000001);
#6170=VECTOR('',#22082,1.60000000000001);
#6171=VECTOR('',#22085,1.60000000000001);
#6172=VECTOR('',#22088,1.60000000000001);
#6173=VECTOR('',#22091,1.60000000000001);
#6174=VECTOR('',#22094,1.60000000000001);
#6175=VECTOR('',#22097,1.60000000000001);
#6176=VECTOR('',#22100,1.60000000000001);
#6177=VECTOR('',#22103,1.60000000000001);
#6178=VECTOR('',#22106,1.60000000000001);
#6179=VECTOR('',#22111,1.59999999999791);
#6180=VECTOR('',#22116,1000.);
#6181=VECTOR('',#22119,1.22111388749974);
#6182=VECTOR('',#22120,1000.);
#6183=VECTOR('',#22123,1.22111388749974);
#6184=VECTOR('',#22126,1.22111388749974);
#6185=VECTOR('',#22129,1.22111388749974);
#6186=VECTOR('',#22132,1.22111388749974);
#6187=VECTOR('',#22135,1.22111388749974);
#6188=VECTOR('',#22138,1.22111388749974);
#6189=VECTOR('',#22141,1.22111388749974);
#6190=VECTOR('',#22144,1.22111388749974);
#6191=VECTOR('',#22147,1.22111388749974);
#6192=VECTOR('',#22150,1.22111388749974);
#6193=VECTOR('',#22153,1.22111388749974);
#6194=VECTOR('',#22156,1.22111388749974);
#6195=VECTOR('',#22159,1.22111388749974);
#6196=VECTOR('',#22162,1.22111388749974);
#6197=VECTOR('',#22165,1.22111388749974);
#6198=VECTOR('',#22168,1.22111388749974);
#6199=VECTOR('',#22171,1.22111388749974);
#6200=VECTOR('',#22174,1.22111388749974);
#6201=VECTOR('',#22177,1.22111388749974);
#6202=VECTOR('',#22178,1000.);
#6203=VECTOR('',#22181,8.49999999999999);
#6204=VECTOR('',#22186,8.49999999999999);
#6205=VECTOR('',#22189,8.49999999999999);
#6206=VECTOR('',#22192,7.68810118749996);
#6207=VECTOR('',#22193,1000.);
#6208=VECTOR('',#22196,7.68810118749996);
#6209=VECTOR('',#22199,7.68810118749996);
#6210=VECTOR('',#22202,7.68810118749996);
#6211=VECTOR('',#22205,7.68810118749996);
#6212=VECTOR('',#22208,7.68810118749996);
#6213=VECTOR('',#22211,7.68810118749996);
#6214=VECTOR('',#22214,7.68810118749996);
#6215=VECTOR('',#22217,8.10000000000001);
#6216=VECTOR('',#22222,8.10000000000001);
#6217=VECTOR('',#22225,8.10000000000001);
#6218=VECTOR('',#22228,8.10000000000001);
#6219=VECTOR('',#22229,1000.);
#6220=VECTOR('',#22236,1000.);
#6221=VECTOR('',#22237,1000.);
#6222=VECTOR('',#22238,1000.);
#6223=VECTOR('',#22241,1000.);
#6224=VECTOR('',#22242,1000.);
#6225=VECTOR('',#22245,1000.);
#6226=VECTOR('',#22246,1000.);
#6227=VECTOR('',#22249,1000.);
#6228=VECTOR('',#22250,1000.);
#6229=VECTOR('',#22253,1000.);
#6230=VECTOR('',#22254,1000.);
#6231=VECTOR('',#22255,1000.);
#6232=VECTOR('',#22260,1000.);
#6233=VECTOR('',#22261,1000.);
#6234=VECTOR('',#22262,1000.);
#6235=VECTOR('',#22265,1000.);
#6236=VECTOR('',#22268,1000.);
#6237=VECTOR('',#22269,1000.);
#6238=VECTOR('',#22272,1000.);
#6239=VECTOR('',#22273,1000.);
#6240=VECTOR('',#22274,1000.);
#6241=VECTOR('',#22279,1000.);
#6242=VECTOR('',#22280,1000.);
#6243=VECTOR('',#22281,1000.);
#6244=VECTOR('',#22284,1000.);
#6245=VECTOR('',#22287,1000.);
#6246=VECTOR('',#22288,1000.);
#6247=VECTOR('',#22291,1000.);
#6248=VECTOR('',#22292,1000.);
#6249=VECTOR('',#22293,1000.);
#6250=VECTOR('',#22300,1000.);
#6251=VECTOR('',#22301,1000.);
#6252=VECTOR('',#22302,1000.);
#6253=VECTOR('',#22305,1000.);
#6254=VECTOR('',#22308,1000.);
#6255=VECTOR('',#22309,1000.);
#6256=VECTOR('',#22324,12.);
#6257=VECTOR('',#22337,8.10000000000001);
#6258=VECTOR('',#22352,14.);
#6259=VECTOR('',#22373,1000.);
#6260=VECTOR('',#22374,1000.);
#6261=VECTOR('',#22375,1000.);
#6262=VECTOR('',#22376,1000.);
#6263=VECTOR('',#22379,1000.);
#6264=VECTOR('',#22388,6.00000000000001);
#6265=VECTOR('',#22393,1000.);
#6266=VECTOR('',#22418,4.75);
#6267=VECTOR('',#22425,7.00000000000001);
#6268=VECTOR('',#22446,10.);
#6269=VECTOR('',#22481,1.2500000000005);
#6270=VECTOR('',#22488,1.25000000000059);
#6271=VECTOR('',#22497,1.25000000000024);
#6272=VECTOR('',#22506,1.24999999999999);
#6273=VECTOR('',#22513,6.00000000000001);
#6274=VECTOR('',#22518,1000.);
#6275=VECTOR('',#22519,1000.);
#6276=VECTOR('',#22520,1000.);
#6277=VECTOR('',#22521,1000.);
#6278=VECTOR('',#22524,1000.);
#6279=VECTOR('',#22525,1000.);
#6280=VECTOR('',#22526,1000.);
#6281=VECTOR('',#22529,1000.);
#6282=VECTOR('',#22530,1000.);
#6283=VECTOR('',#22531,1000.);
#6284=VECTOR('',#22534,1000.);
#6285=VECTOR('',#22535,1000.);
#6286=VECTOR('',#22536,1000.);
#6287=VECTOR('',#22539,1000.);
#6288=VECTOR('',#22540,1000.);
#6289=VECTOR('',#22541,1000.);
#6290=VECTOR('',#22544,1000.);
#6291=VECTOR('',#22545,1000.);
#6292=VECTOR('',#22546,1000.);
#6293=VECTOR('',#22549,1000.);
#6294=VECTOR('',#22550,1000.);
#6295=VECTOR('',#22551,1000.);
#6296=VECTOR('',#22554,1000.);
#6297=VECTOR('',#22555,1000.);
#6298=VECTOR('',#22556,1000.);
#6299=VECTOR('',#22559,1000.);
#6300=VECTOR('',#22560,1000.);
#6301=VECTOR('',#22561,1000.);
#6302=VECTOR('',#22564,1000.);
#6303=VECTOR('',#22565,1000.);
#6304=VECTOR('',#22566,1000.);
#6305=VECTOR('',#22569,1000.);
#6306=VECTOR('',#22570,1000.);
#6307=VECTOR('',#22571,1000.);
#6308=VECTOR('',#22574,1000.);
#6309=VECTOR('',#22575,1000.);
#6310=VECTOR('',#22576,1000.);
#6311=VECTOR('',#22579,1000.);
#6312=VECTOR('',#22580,1000.);
#6313=VECTOR('',#22581,1000.);
#6314=VECTOR('',#22584,1000.);
#6315=VECTOR('',#22585,1000.);
#6316=VECTOR('',#22586,1000.);
#6317=VECTOR('',#22589,1000.);
#6318=VECTOR('',#22590,1000.);
#6319=VECTOR('',#22591,1000.);
#6320=VECTOR('',#22594,1000.);
#6321=VECTOR('',#22595,1000.);
#6322=VECTOR('',#22596,1000.);
#6323=VECTOR('',#22599,1000.);
#6324=VECTOR('',#22600,1000.);
#6325=VECTOR('',#22601,1000.);
#6326=VECTOR('',#22604,1000.);
#6327=VECTOR('',#22605,1000.);
#6328=VECTOR('',#22606,1000.);
#6329=VECTOR('',#22609,1000.);
#6330=VECTOR('',#22610,1000.);
#6331=VECTOR('',#22611,1000.);
#6332=VECTOR('',#22614,1000.);
#6333=VECTOR('',#22615,1000.);
#6334=VECTOR('',#22616,1000.);
#6335=VECTOR('',#22619,1000.);
#6336=VECTOR('',#22620,1000.);
#6337=VECTOR('',#22621,1000.);
#6338=VECTOR('',#22624,1000.);
#6339=VECTOR('',#22625,1000.);
#6340=VECTOR('',#22626,1000.);
#6341=VECTOR('',#22629,1000.);
#6342=VECTOR('',#22630,1000.);
#6343=VECTOR('',#22631,1000.);
#6344=VECTOR('',#22634,1000.);
#6345=VECTOR('',#22635,1000.);
#6346=VECTOR('',#22636,1000.);
#6347=VECTOR('',#22639,1000.);
#6348=VECTOR('',#22640,1000.);
#6349=VECTOR('',#22641,1000.);
#6350=VECTOR('',#22644,1000.);
#6351=VECTOR('',#22645,1000.);
#6352=VECTOR('',#22646,1000.);
#6353=VECTOR('',#22649,1000.);
#6354=VECTOR('',#22650,1000.);
#6355=VECTOR('',#22651,1000.);
#6356=VECTOR('',#22654,1000.);
#6357=VECTOR('',#22655,1000.);
#6358=VECTOR('',#22656,1000.);
#6359=VECTOR('',#22659,1000.);
#6360=VECTOR('',#22660,1000.);
#6361=VECTOR('',#22661,1000.);
#6362=VECTOR('',#22664,1000.);
#6363=VECTOR('',#22665,1000.);
#6364=VECTOR('',#22666,1000.);
#6365=VECTOR('',#22669,1000.);
#6366=VECTOR('',#22670,1000.);
#6367=VECTOR('',#22671,1000.);
#6368=VECTOR('',#22674,1000.);
#6369=VECTOR('',#22675,1000.);
#6370=VECTOR('',#22676,1000.);
#6371=VECTOR('',#22679,1000.);
#6372=VECTOR('',#22680,1000.);
#6373=VECTOR('',#22681,1000.);
#6374=VECTOR('',#22684,1000.);
#6375=VECTOR('',#22685,1000.);
#6376=VECTOR('',#22686,1000.);
#6377=VECTOR('',#22689,1000.);
#6378=VECTOR('',#22690,1000.);
#6379=VECTOR('',#22691,1000.);
#6380=VECTOR('',#22694,1000.);
#6381=VECTOR('',#22695,1000.);
#6382=VECTOR('',#22696,1000.);
#6383=VECTOR('',#22699,1000.);
#6384=VECTOR('',#22700,1000.);
#6385=VECTOR('',#22701,1000.);
#6386=VECTOR('',#22704,1000.);
#6387=VECTOR('',#22705,1000.);
#6388=VECTOR('',#22706,1000.);
#6389=VECTOR('',#22709,1000.);
#6390=VECTOR('',#22710,1000.);
#6391=VECTOR('',#22711,1000.);
#6392=VECTOR('',#22714,1000.);
#6393=VECTOR('',#22715,1000.);
#6394=VECTOR('',#22716,1000.);
#6395=VECTOR('',#22719,1000.);
#6396=VECTOR('',#22720,1000.);
#6397=VECTOR('',#22721,1000.);
#6398=VECTOR('',#22724,1000.);
#6399=VECTOR('',#22725,1000.);
#6400=VECTOR('',#22726,1000.);
#6401=VECTOR('',#22729,1000.);
#6402=VECTOR('',#22730,1000.);
#6403=VECTOR('',#22731,1000.);
#6404=VECTOR('',#22734,1000.);
#6405=VECTOR('',#22735,1000.);
#6406=VECTOR('',#22736,1000.);
#6407=VECTOR('',#22739,1000.);
#6408=VECTOR('',#22740,1000.);
#6409=VECTOR('',#22741,1000.);
#6410=VECTOR('',#22744,1000.);
#6411=VECTOR('',#22745,1000.);
#6412=VECTOR('',#22746,1000.);
#6413=VECTOR('',#22749,1000.);
#6414=VECTOR('',#22750,1000.);
#6415=VECTOR('',#22751,1000.);
#6416=VECTOR('',#22754,1000.);
#6417=VECTOR('',#22755,1000.);
#6418=VECTOR('',#22756,1000.);
#6419=VECTOR('',#22759,1000.);
#6420=VECTOR('',#22760,1000.);
#6421=VECTOR('',#22761,1000.);
#6422=VECTOR('',#22764,1000.);
#6423=VECTOR('',#22765,1000.);
#6424=VECTOR('',#22766,1000.);
#6425=VECTOR('',#22769,1000.);
#6426=VECTOR('',#22770,1000.);
#6427=VECTOR('',#22771,1000.);
#6428=VECTOR('',#22774,1000.);
#6429=VECTOR('',#22775,1000.);
#6430=VECTOR('',#22776,1000.);
#6431=VECTOR('',#22779,1000.);
#6432=VECTOR('',#22780,1000.);
#6433=VECTOR('',#22781,1000.);
#6434=VECTOR('',#22784,1000.);
#6435=VECTOR('',#22785,1000.);
#6436=VECTOR('',#22786,1000.);
#6437=VECTOR('',#22789,1000.);
#6438=VECTOR('',#22790,1000.);
#6439=VECTOR('',#22791,1000.);
#6440=VECTOR('',#22794,1000.);
#6441=VECTOR('',#22795,1000.);
#6442=VECTOR('',#22796,1000.);
#6443=VECTOR('',#22799,1000.);
#6444=VECTOR('',#22800,1000.);
#6445=VECTOR('',#22801,1000.);
#6446=VECTOR('',#22804,1000.);
#6447=VECTOR('',#22805,1000.);
#6448=VECTOR('',#22806,1000.);
#6449=VECTOR('',#22809,1000.);
#6450=VECTOR('',#22810,1000.);
#6451=VECTOR('',#22811,1000.);
#6452=VECTOR('',#22814,1000.);
#6453=VECTOR('',#22815,1000.);
#6454=VECTOR('',#22816,1000.);
#6455=VECTOR('',#22819,1000.);
#6456=VECTOR('',#22820,1000.);
#6457=VECTOR('',#22821,1000.);
#6458=VECTOR('',#22824,1000.);
#6459=VECTOR('',#22825,1000.);
#6460=VECTOR('',#22826,1000.);
#6461=VECTOR('',#22829,1000.);
#6462=VECTOR('',#22830,1000.);
#6463=VECTOR('',#22831,1000.);
#6464=VECTOR('',#22834,1000.);
#6465=VECTOR('',#22835,1000.);
#6466=VECTOR('',#22836,1000.);
#6467=VECTOR('',#22839,1000.);
#6468=VECTOR('',#22840,1000.);
#6469=VECTOR('',#22841,1000.);
#6470=VECTOR('',#22844,1000.);
#6471=VECTOR('',#22845,1000.);
#6472=VECTOR('',#22846,1000.);
#6473=VECTOR('',#22849,1000.);
#6474=VECTOR('',#22850,1000.);
#6475=VECTOR('',#22851,1000.);
#6476=VECTOR('',#22854,1000.);
#6477=VECTOR('',#22855,1000.);
#6478=VECTOR('',#22856,1000.);
#6479=VECTOR('',#22859,1000.);
#6480=VECTOR('',#22860,1000.);
#6481=VECTOR('',#22861,1000.);
#6482=VECTOR('',#22864,1000.);
#6483=VECTOR('',#22865,1000.);
#6484=VECTOR('',#22866,1000.);
#6485=VECTOR('',#22869,1000.);
#6486=VECTOR('',#22870,1000.);
#6487=VECTOR('',#22871,1000.);
#6488=VECTOR('',#22874,1000.);
#6489=VECTOR('',#22875,1000.);
#6490=VECTOR('',#22876,1000.);
#6491=VECTOR('',#22879,1000.);
#6492=VECTOR('',#22880,1000.);
#6493=VECTOR('',#22881,1000.);
#6494=VECTOR('',#22884,1000.);
#6495=VECTOR('',#22885,1000.);
#6496=VECTOR('',#22886,1000.);
#6497=VECTOR('',#22889,1000.);
#6498=VECTOR('',#22890,1000.);
#6499=VECTOR('',#22891,1000.);
#6500=VECTOR('',#22894,1000.);
#6501=VECTOR('',#22895,1000.);
#6502=VECTOR('',#22896,1000.);
#6503=VECTOR('',#22899,1000.);
#6504=VECTOR('',#22900,1000.);
#6505=VECTOR('',#22901,1000.);
#6506=VECTOR('',#22904,1000.);
#6507=VECTOR('',#22905,1000.);
#6508=VECTOR('',#22906,1000.);
#6509=VECTOR('',#22909,1000.);
#6510=VECTOR('',#22910,1000.);
#6511=VECTOR('',#22911,1000.);
#6512=VECTOR('',#22914,1000.);
#6513=VECTOR('',#22915,1000.);
#6514=VECTOR('',#22916,1000.);
#6515=VECTOR('',#22919,1000.);
#6516=VECTOR('',#22920,1000.);
#6517=VECTOR('',#22921,1000.);
#6518=VECTOR('',#22924,1000.);
#6519=VECTOR('',#22925,1000.);
#6520=VECTOR('',#22926,1000.);
#6521=VECTOR('',#22929,1000.);
#6522=VECTOR('',#22930,1000.);
#6523=VECTOR('',#22931,1000.);
#6524=VECTOR('',#22934,1000.);
#6525=VECTOR('',#22935,1000.);
#6526=VECTOR('',#22936,1000.);
#6527=VECTOR('',#22939,1000.);
#6528=VECTOR('',#22940,1000.);
#6529=VECTOR('',#22941,1000.);
#6530=VECTOR('',#22944,1000.);
#6531=VECTOR('',#22945,1000.);
#6532=VECTOR('',#22946,1000.);
#6533=VECTOR('',#22949,1000.);
#6534=VECTOR('',#22950,1000.);
#6535=VECTOR('',#22951,1000.);
#6536=VECTOR('',#22954,1000.);
#6537=VECTOR('',#22955,1000.);
#6538=VECTOR('',#22956,1000.);
#6539=VECTOR('',#22959,1000.);
#6540=VECTOR('',#22960,1000.);
#6541=VECTOR('',#22961,1000.);
#6542=VECTOR('',#22964,1000.);
#6543=VECTOR('',#22965,1000.);
#6544=VECTOR('',#22986,3.99999999999999);
#6545=VECTOR('',#22987,1000.);
#6546=VECTOR('',#22988,1000.);
#6547=VECTOR('',#22991,1000.);
#6548=VECTOR('',#22992,1000.);
#6549=VECTOR('',#22997,1000.);
#6550=VECTOR('',#23008,1.60000000000001);
#6551=VECTOR('',#23013,2.);
#6552=VECTOR('',#23018,3.99999999999999);
#6553=VECTOR('',#23025,3.6);
#6554=VECTOR('',#23030,3.99999999999999);
#6555=VECTOR('',#23043,1.4);
#6556=VECTOR('',#23048,1000.);
#6557=VECTOR('',#23057,1.4);
#6558=VECTOR('',#23062,1000.);
#6559=VECTOR('',#23063,1000.);
#6560=VECTOR('',#23064,1000.);
#6561=VECTOR('',#23065,1000.);
#6562=VECTOR('',#23066,1000.);
#6563=VECTOR('',#23067,1000.);
#6564=VECTOR('',#23070,1000.);
#6565=VECTOR('',#23071,1000.);
#6566=VECTOR('',#23072,1000.);
#6567=VECTOR('',#23075,1000.);
#6568=VECTOR('',#23076,1000.);
#6569=VECTOR('',#23079,1000.);
#6570=VECTOR('',#23080,1000.);
#6571=VECTOR('',#23083,1000.);
#6572=VECTOR('',#23084,1000.);
#6573=VECTOR('',#23087,1000.);
#6574=VECTOR('',#23088,1000.);
#6575=VECTOR('',#23091,1000.);
#6576=VECTOR('',#23094,1000.);
#6577=VECTOR('',#23095,1000.);
#6578=VECTOR('',#23096,1000.);
#6579=VECTOR('',#23097,1000.);
#6580=VECTOR('',#23098,1000.);
#6581=VECTOR('',#23099,1000.);
#6582=VECTOR('',#23100,1000.);
#6583=VECTOR('',#23101,1000.);
#6584=VECTOR('',#23102,1000.);
#6585=VECTOR('',#23105,1000.);
#6586=VECTOR('',#23106,1000.);
#6587=VECTOR('',#23109,1000.);
#6588=VECTOR('',#23110,1000.);
#6589=VECTOR('',#23113,1000.);
#6590=VECTOR('',#23114,1000.);
#6591=VECTOR('',#23117,1000.);
#6592=VECTOR('',#23118,1000.);
#6593=VECTOR('',#23121,1000.);
#6594=VECTOR('',#23122,1000.);
#6595=VECTOR('',#23123,1000.);
#6596=VECTOR('',#23124,1000.);
#6597=VECTOR('',#23125,1000.);
#6598=VECTOR('',#23128,1000.);
#6599=VECTOR('',#23129,1000.);
#6600=VECTOR('',#23132,1000.);
#6601=VECTOR('',#23133,1000.);
#6602=VECTOR('',#23134,1000.);
#6603=VECTOR('',#23135,1000.);
#6604=VECTOR('',#23136,1000.);
#6605=VECTOR('',#23139,1000.);
#6606=VECTOR('',#23140,1000.);
#6607=VECTOR('',#23141,1000.);
#6608=VECTOR('',#23144,1000.);
#6609=VECTOR('',#23145,1000.);
#6610=VECTOR('',#23146,1000.);
#6611=VECTOR('',#23149,1000.);
#6612=VECTOR('',#23150,1000.);
#6613=VECTOR('',#23151,1000.);
#6614=VECTOR('',#23152,1000.);
#6615=VECTOR('',#23155,1000.);
#6616=VECTOR('',#23156,1000.);
#6617=VECTOR('',#23157,1000.);
#6618=VECTOR('',#23160,1000.);
#6619=VECTOR('',#23161,1000.);
#6620=VECTOR('',#23162,1000.);
#6621=VECTOR('',#23163,1000.);
#6622=VECTOR('',#23166,1000.);
#6623=VECTOR('',#23167,1000.);
#6624=VECTOR('',#23168,1000.);
#6625=VECTOR('',#23169,1000.);
#6626=VECTOR('',#23172,1000.);
#6627=VECTOR('',#23173,1000.);
#6628=VECTOR('',#23174,1000.);
#6629=VECTOR('',#23175,1000.);
#6630=VECTOR('',#23176,1000.);
#6631=VECTOR('',#23189,1.6);
#6632=VECTOR('',#23194,1.6);
#6633=VECTOR('',#23197,1000.);
#6634=VECTOR('',#23198,1000.);
#6635=VECTOR('',#23199,1000.);
#6636=VECTOR('',#23200,1000.);
#6637=VECTOR('',#23201,1000.);
#6638=VECTOR('',#23202,1000.);
#6639=VECTOR('',#23205,1000.);
#6640=VECTOR('',#23206,1000.);
#6641=VECTOR('',#23207,1000.);
#6642=VECTOR('',#23210,1000.);
#6643=VECTOR('',#23211,1000.);
#6644=VECTOR('',#23212,1000.);
#6645=VECTOR('',#23213,1000.);
#6646=VECTOR('',#23214,1000.);
#6647=VECTOR('',#23217,1000.);
#6648=VECTOR('',#23218,1000.);
#6649=VECTOR('',#23223,1000.);
#6650=VECTOR('',#23224,1000.);
#6651=VECTOR('',#23227,1000.);
#6652=VECTOR('',#23228,1000.);
#6653=VECTOR('',#23229,1000.);
#6654=VECTOR('',#23230,1000.);
#6655=VECTOR('',#23237,1000.);
#6656=VECTOR('',#23238,1000.);
#6657=VECTOR('',#23239,1000.);
#6658=VECTOR('',#23240,1000.);
#6659=VECTOR('',#23247,1000.);
#6660=VECTOR('',#23248,1000.);
#6661=VECTOR('',#23249,1000.);
#6662=VECTOR('',#23252,2.);
#6663=VECTOR('',#23255,2.);
#6664=VECTOR('',#23258,1000.);
#6665=VECTOR('',#23261,1000.);
#6666=VECTOR('',#23262,1000.);
#6667=VECTOR('',#23263,1000.);
#6668=VECTOR('',#23264,1000.);
#6669=VECTOR('',#23265,1000.);
#6670=VECTOR('',#23268,1000.);
#6671=VECTOR('',#23281,1.6);
#6672=VECTOR('',#23286,1.6);
#6673=VECTOR('',#23289,1000.);
#6674=VECTOR('',#23290,1000.);
#6675=VECTOR('',#23291,1000.);
#6676=VECTOR('',#23292,1000.);
#6677=VECTOR('',#23293,1000.);
#6678=VECTOR('',#23296,1000.);
#6679=VECTOR('',#23297,1000.);
#6680=VECTOR('',#23300,1000.);
#6681=VECTOR('',#23301,1000.);
#6682=VECTOR('',#23302,1000.);
#6683=VECTOR('',#23303,1000.);
#6684=VECTOR('',#23306,1000.);
#6685=VECTOR('',#23307,1000.);
#6686=VECTOR('',#23312,1000.);
#6687=VECTOR('',#23313,1000.);
#6688=VECTOR('',#23314,1000.);
#6689=VECTOR('',#23317,1000.);
#6690=VECTOR('',#23318,1000.);
#6691=VECTOR('',#23319,1000.);
#6692=VECTOR('',#23320,1000.);
#6693=VECTOR('',#23321,1000.);
#6694=VECTOR('',#23322,1000.);
#6695=VECTOR('',#23325,1000.);
#6696=VECTOR('',#23326,1000.);
#6697=VECTOR('',#23327,1000.);
#6698=VECTOR('',#23330,1000.);
#6699=VECTOR('',#23331,1000.);
#6700=VECTOR('',#23332,1000.);
#6701=VECTOR('',#23335,1000.);
#6702=VECTOR('',#23336,1000.);
#6703=VECTOR('',#23337,1000.);
#6704=VECTOR('',#23340,1000.);
#6705=VECTOR('',#23343,1000.);
#6706=VECTOR('',#23346,1000.);
#6707=VECTOR('',#23347,1000.);
#6708=VECTOR('',#23352,1000.);
#6709=VECTOR('',#23371,4.);
#6710=VECTOR('',#23374,4.);
#6711=VECTOR('',#23377,1.6);
#6712=VECTOR('',#23378,1000.);
#6713=VECTOR('',#23383,1.6);
#6714=VECTOR('',#23386,1.6);
#6715=VECTOR('',#23389,1.6);
#6716=VECTOR('',#23392,1.6);
#6717=VECTOR('',#23395,1.6);
#6718=VECTOR('',#23398,1.6);
#6719=VECTOR('',#23401,1.6);
#6720=VECTOR('',#23404,1.6);
#6721=VECTOR('',#23407,1.6);
#6722=VECTOR('',#23410,1.6);
#6723=VECTOR('',#23413,1.6);
#6724=VECTOR('',#23416,1.6);
#6725=VECTOR('',#23419,1.6);
#6726=VECTOR('',#23424,1.22111388750008);
#6727=VECTOR('',#23425,1000.);
#6728=VECTOR('',#23428,1.22111388750008);
#6729=VECTOR('',#23431,1.22111388750008);
#6730=VECTOR('',#23434,1.22111388750008);
#6731=VECTOR('',#23437,1.22111388750008);
#6732=VECTOR('',#23440,1.22111388750008);
#6733=VECTOR('',#23443,1.22111388750008);
#6734=VECTOR('',#23446,1.22111388750008);
#6735=VECTOR('',#23449,1.22111388750008);
#6736=VECTOR('',#23452,1.22111388750008);
#6737=VECTOR('',#23455,1.22111388750008);
#6738=VECTOR('',#23458,1.22111388750008);
#6739=VECTOR('',#23461,1.22111388750008);
#6740=VECTOR('',#23464,1.22111388750008);
#6741=VECTOR('',#23465,1000.);
#6742=VECTOR('',#23470,1.60000000000001);
#6743=VECTOR('',#23477,1.49172584788676);
#6744=VECTOR('',#23484,1.04190416256385);
#6745=VECTOR('',#23529,3.25);
#6746=VECTOR('',#23532,12.);
#6747=VECTOR('',#23549,1000.);
#6748=VECTOR('',#23550,1000.);
#6749=VECTOR('',#23551,1000.);
#6750=VECTOR('',#23554,1000.);
#6751=VECTOR('',#23555,1000.);
#6752=VECTOR('',#23558,1000.);
#6753=VECTOR('',#23567,1.6);
#6754=VECTOR('',#23572,2.);
#6755=VECTOR('',#23579,3.6);
#6756=VECTOR('',#23606,5.);
#6757=VECTOR('',#23611,7.);
#6758=VECTOR('',#23616,1000.);
#6759=VECTOR('',#23619,1000.);
#6760=VECTOR('',#23624,1.6);
#6761=VECTOR('',#23629,1000.);
#6762=VECTOR('',#23630,1000.);
#6763=VECTOR('',#23631,1000.);
#6764=VECTOR('',#23632,1000.);
#6765=VECTOR('',#23633,1000.);
#6766=VECTOR('',#23634,1000.);
#6767=VECTOR('',#23635,1000.);
#6768=VECTOR('',#23638,1000.);
#6769=VECTOR('',#23639,1000.);
#6770=VECTOR('',#23640,1000.);
#6771=VECTOR('',#23641,1000.);
#6772=VECTOR('',#23642,1000.);
#6773=VECTOR('',#23643,1000.);
#6774=VECTOR('',#23648,1000.);
#6775=VECTOR('',#23651,1000.);
#6776=VECTOR('',#23654,1000.);
#6777=VECTOR('',#23655,1000.);
#6778=VECTOR('',#23656,1000.);
#6779=VECTOR('',#23657,1000.);
#6780=VECTOR('',#23658,1000.);
#6781=VECTOR('',#23659,1000.);
#6782=VECTOR('',#23660,1000.);
#6783=VECTOR('',#23661,1000.);
#6784=VECTOR('',#23662,1000.);
#6785=VECTOR('',#23665,1000.);
#6786=VECTOR('',#23666,1000.);
#6787=VECTOR('',#23667,1000.);
#6788=VECTOR('',#23668,1000.);
#6789=VECTOR('',#23671,1000.);
#6790=VECTOR('',#23672,1000.);
#6791=VECTOR('',#23673,1000.);
#6792=VECTOR('',#23674,1000.);
#6793=VECTOR('',#23675,1000.);
#6794=VECTOR('',#23676,1000.);
#6795=VECTOR('',#23679,1000.);
#6796=VECTOR('',#23682,1000.);
#6797=VECTOR('',#23685,1000.);
#6798=VECTOR('',#23688,1000.);
#6799=VECTOR('',#23691,1000.);
#6800=VECTOR('',#23694,1000.);
#6801=VECTOR('',#23697,1000.);
#6802=VECTOR('',#23700,1000.);
#6803=VECTOR('',#23703,1000.);
#6804=VECTOR('',#23706,1000.);
#6805=VECTOR('',#23709,1000.);
#6806=VECTOR('',#23712,1000.);
#6807=VECTOR('',#23715,1000.);
#6808=VECTOR('',#23720,1000.);
#6809=VECTOR('',#23723,1000.);
#6810=VECTOR('',#23724,1000.);
#6811=VECTOR('',#23727,1000.);
#6812=VECTOR('',#23732,1000.);
#6813=VECTOR('',#23735,1000.);
#6814=VECTOR('',#23738,1000.);
#6815=VECTOR('',#23741,1000.);
#6816=VECTOR('',#23742,1000.);
#6817=VECTOR('',#23747,1000.);
#6818=VECTOR('',#23750,1000.);
#6819=VECTOR('',#23751,1000.);
#6820=VECTOR('',#23754,1000.);
#6821=VECTOR('',#23761,1000.);
#6822=VECTOR('',#23764,1000.);
#6823=VECTOR('',#23765,1000.);
#6824=VECTOR('',#23768,1000.);
#6825=VECTOR('',#23769,1000.);
#6826=VECTOR('',#23772,1000.);
#6827=VECTOR('',#23783,1000.);
#6828=VECTOR('',#23786,1000.);
#6829=VECTOR('',#23787,1000.);
#6830=VECTOR('',#23790,1000.);
#6831=VECTOR('',#23791,1000.);
#6832=VECTOR('',#23794,1000.);
#6833=VECTOR('',#23809,1000.);
#6834=VECTOR('',#23810,1000.);
#6835=VECTOR('',#23811,1000.);
#6836=VECTOR('',#23814,1000.);
#6837=VECTOR('',#23815,1000.);
#6838=VECTOR('',#23818,1000.);
#6839=VECTOR('',#23819,1000.);
#6840=VECTOR('',#23822,1000.);
#6841=VECTOR('',#23823,1000.);
#6842=VECTOR('',#23826,1000.);
#6843=VECTOR('',#23827,1000.);
#6844=VECTOR('',#23830,1000.);
#6845=VECTOR('',#23833,1000.);
#6846=VECTOR('',#23834,1000.);
#6847=VECTOR('',#23835,1000.);
#6848=VECTOR('',#23836,1000.);
#6849=VECTOR('',#23837,1000.);
#6850=VECTOR('',#23838,1000.);
#6851=VECTOR('',#23865,4.);
#6852=VECTOR('',#23872,1.6);
#6853=VECTOR('',#23877,1000.);
#6854=VECTOR('',#23878,1000.);
#6855=VECTOR('',#23879,1000.);
#6856=VECTOR('',#23880,1000.);
#6857=VECTOR('',#23885,1000.);
#6858=VECTOR('',#23890,1000.);
#6859=VECTOR('',#23891,1000.);
#6860=VECTOR('',#23892,1000.);
#6861=VECTOR('',#23895,1000.);
#6862=VECTOR('',#23896,1000.);
#6863=VECTOR('',#23897,1000.);
#6864=VECTOR('',#23900,1000.);
#6865=VECTOR('',#23901,1000.);
#6866=VECTOR('',#23902,1000.);
#6867=VECTOR('',#23905,1000.);
#6868=VECTOR('',#23906,1000.);
#6869=VECTOR('',#23907,1000.);
#6870=VECTOR('',#23910,1000.);
#6871=VECTOR('',#23911,1000.);
#6872=VECTOR('',#23912,1000.);
#6873=VECTOR('',#23915,1000.);
#6874=VECTOR('',#23916,1000.);
#6875=VECTOR('',#23917,1000.);
#6876=VECTOR('',#23920,1000.);
#6877=VECTOR('',#23921,1000.);
#6878=VECTOR('',#23922,1000.);
#6879=VECTOR('',#23925,1000.);
#6880=VECTOR('',#23926,1000.);
#6881=VECTOR('',#23927,1000.);
#6882=VECTOR('',#23930,1000.);
#6883=VECTOR('',#23931,1000.);
#6884=VECTOR('',#23932,1000.);
#6885=VECTOR('',#23935,1000.);
#6886=VECTOR('',#23936,1000.);
#6887=VECTOR('',#23937,1000.);
#6888=VECTOR('',#23940,1000.);
#6889=VECTOR('',#23941,1000.);
#6890=VECTOR('',#23942,1000.);
#6891=VECTOR('',#23945,1000.);
#6892=VECTOR('',#23946,1000.);
#6893=VECTOR('',#23947,1000.);
#6894=VECTOR('',#23950,1000.);
#6895=VECTOR('',#23951,1000.);
#6896=VECTOR('',#23952,1000.);
#6897=VECTOR('',#23955,1000.);
#6898=VECTOR('',#23956,1000.);
#6899=VECTOR('',#23957,1000.);
#6900=VECTOR('',#23960,1000.);
#6901=VECTOR('',#23961,1000.);
#6902=VECTOR('',#23962,1000.);
#6903=VECTOR('',#23965,1000.);
#6904=VECTOR('',#23966,1000.);
#6905=VECTOR('',#23967,1000.);
#6906=VECTOR('',#23970,1000.);
#6907=VECTOR('',#23971,1000.);
#6908=VECTOR('',#23972,1000.);
#6909=VECTOR('',#23975,1000.);
#6910=VECTOR('',#23976,1000.);
#6911=VECTOR('',#23977,1000.);
#6912=VECTOR('',#23980,1000.);
#6913=VECTOR('',#23981,1000.);
#6914=VECTOR('',#23982,1000.);
#6915=VECTOR('',#23985,1000.);
#6916=VECTOR('',#23986,1000.);
#6917=VECTOR('',#23987,1000.);
#6918=VECTOR('',#23990,1000.);
#6919=VECTOR('',#23991,1000.);
#6920=VECTOR('',#23992,1000.);
#6921=VECTOR('',#23995,1000.);
#6922=VECTOR('',#23996,1000.);
#6923=VECTOR('',#23997,1000.);
#6924=VECTOR('',#24000,1000.);
#6925=VECTOR('',#24001,1000.);
#6926=VECTOR('',#24002,1000.);
#6927=VECTOR('',#24005,1000.);
#6928=VECTOR('',#24006,1000.);
#6929=VECTOR('',#24007,1000.);
#6930=VECTOR('',#24010,1000.);
#6931=VECTOR('',#24011,1000.);
#6932=VECTOR('',#24012,1000.);
#6933=VECTOR('',#24015,1000.);
#6934=VECTOR('',#24016,1000.);
#6935=VECTOR('',#24017,1000.);
#6936=VECTOR('',#24020,1000.);
#6937=VECTOR('',#24021,1000.);
#6938=VECTOR('',#24022,1000.);
#6939=VECTOR('',#24025,1000.);
#6940=VECTOR('',#24026,1000.);
#6941=VECTOR('',#24027,1000.);
#6942=VECTOR('',#24030,1000.);
#6943=VECTOR('',#24031,1000.);
#6944=VECTOR('',#24032,1000.);
#6945=VECTOR('',#24035,1000.);
#6946=VECTOR('',#24036,1000.);
#6947=VECTOR('',#24037,1000.);
#6948=VECTOR('',#24040,1000.);
#6949=VECTOR('',#24041,1000.);
#6950=VECTOR('',#24042,1000.);
#6951=VECTOR('',#24045,1000.);
#6952=VECTOR('',#24046,1000.);
#6953=VECTOR('',#24047,1000.);
#6954=VECTOR('',#24050,1000.);
#6955=VECTOR('',#24051,1000.);
#6956=VECTOR('',#24052,1000.);
#6957=VECTOR('',#24055,1000.);
#6958=VECTOR('',#24056,1000.);
#6959=VECTOR('',#24057,1000.);
#6960=VECTOR('',#24060,1000.);
#6961=VECTOR('',#24061,1000.);
#6962=VECTOR('',#24062,1000.);
#6963=VECTOR('',#24065,1000.);
#6964=VECTOR('',#24066,1000.);
#6965=VECTOR('',#24067,1000.);
#6966=VECTOR('',#24070,1000.);
#6967=VECTOR('',#24071,1000.);
#6968=VECTOR('',#24072,1000.);
#6969=VECTOR('',#24075,1000.);
#6970=VECTOR('',#24076,1000.);
#6971=VECTOR('',#24077,1000.);
#6972=VECTOR('',#24084,1000.);
#6973=VECTOR('',#24087,1000.);
#6974=VECTOR('',#24088,1000.);
#6975=VECTOR('',#24089,1000.);
#6976=VECTOR('',#24092,1000.);
#6977=VECTOR('',#24093,1000.);
#6978=VECTOR('',#24106,1.49172584788676);
#6979=VECTOR('',#24111,1000.);
#6980=VECTOR('',#24112,1000.);
#6981=VECTOR('',#24113,1000.);
#6982=VECTOR('',#24114,1000.);
#6983=VECTOR('',#24119,1000.);
#6984=VECTOR('',#24124,1000.);
#6985=VECTOR('',#24125,1000.);
#6986=VECTOR('',#24126,1000.);
#6987=VECTOR('',#24129,1000.);
#6988=VECTOR('',#24130,1000.);
#6989=VECTOR('',#24131,1000.);
#6990=VECTOR('',#24134,1000.);
#6991=VECTOR('',#24135,1000.);
#6992=VECTOR('',#24136,1000.);
#6993=VECTOR('',#24139,1000.);
#6994=VECTOR('',#24140,1000.);
#6995=VECTOR('',#24141,1000.);
#6996=VECTOR('',#24148,1000.);
#6997=VECTOR('',#24151,1000.);
#6998=VECTOR('',#24152,1000.);
#6999=VECTOR('',#24153,1000.);
#7000=VECTOR('',#24156,1000.);
#7001=VECTOR('',#24157,1000.);
#7002=VECTOR('',#24158,1000.);
#7003=VECTOR('',#24161,1000.);
#7004=VECTOR('',#24162,1000.);
#7005=VECTOR('',#24163,1000.);
#7006=VERTEX_POINT('',#24197);
#7007=VERTEX_POINT('',#24198);
#7008=VERTEX_POINT('',#24200);
#7009=VERTEX_POINT('',#24202);
#7010=VERTEX_POINT('',#24205);
#7011=VERTEX_POINT('',#24207);
#7012=VERTEX_POINT('',#24209);
#7013=VERTEX_POINT('',#24211);
#7014=VERTEX_POINT('',#24213);
#7015=VERTEX_POINT('',#24215);
#7016=VERTEX_POINT('',#24217);
#7017=VERTEX_POINT('',#24219);
#7018=VERTEX_POINT('',#24221);
#7019=VERTEX_POINT('',#24223);
#7020=VERTEX_POINT('',#24225);
#7021=VERTEX_POINT('',#24227);
#7022=VERTEX_POINT('',#24229);
#7023=VERTEX_POINT('',#24231);
#7024=VERTEX_POINT('',#24233);
#7025=VERTEX_POINT('',#24235);
#7026=VERTEX_POINT('',#24237);
#7027=VERTEX_POINT('',#24239);
#7028=VERTEX_POINT('',#24241);
#7029=VERTEX_POINT('',#24243);
#7030=VERTEX_POINT('',#24245);
#7031=VERTEX_POINT('',#24247);
#7032=VERTEX_POINT('',#24249);
#7033=VERTEX_POINT('',#24251);
#7034=VERTEX_POINT('',#24253);
#7035=VERTEX_POINT('',#24255);
#7036=VERTEX_POINT('',#24257);
#7037=VERTEX_POINT('',#24258);
#7038=VERTEX_POINT('',#24260);
#7039=VERTEX_POINT('',#24262);
#7040=VERTEX_POINT('',#24265);
#7041=VERTEX_POINT('',#24266);
#7042=VERTEX_POINT('',#24268);
#7043=VERTEX_POINT('',#24270);
#7044=VERTEX_POINT('',#24273);
#7045=VERTEX_POINT('',#24274);
#7046=VERTEX_POINT('',#24276);
#7047=VERTEX_POINT('',#24278);
#7048=VERTEX_POINT('',#24281);
#7049=VERTEX_POINT('',#24282);
#7050=VERTEX_POINT('',#24284);
#7051=VERTEX_POINT('',#24286);
#7052=VERTEX_POINT('',#24289);
#7053=VERTEX_POINT('',#24290);
#7054=VERTEX_POINT('',#24292);
#7055=VERTEX_POINT('',#24294);
#7056=VERTEX_POINT('',#24297);
#7057=VERTEX_POINT('',#24298);
#7058=VERTEX_POINT('',#24300);
#7059=VERTEX_POINT('',#24302);
#7060=VERTEX_POINT('',#24305);
#7061=VERTEX_POINT('',#24306);
#7062=VERTEX_POINT('',#24308);
#7063=VERTEX_POINT('',#24310);
#7064=VERTEX_POINT('',#24313);
#7065=VERTEX_POINT('',#24314);
#7066=VERTEX_POINT('',#24316);
#7067=VERTEX_POINT('',#24318);
#7068=VERTEX_POINT('',#24321);
#7069=VERTEX_POINT('',#24322);
#7070=VERTEX_POINT('',#24324);
#7071=VERTEX_POINT('',#24326);
#7072=VERTEX_POINT('',#24329);
#7073=VERTEX_POINT('',#24330);
#7074=VERTEX_POINT('',#24332);
#7075=VERTEX_POINT('',#24334);
#7076=VERTEX_POINT('',#24337);
#7077=VERTEX_POINT('',#24338);
#7078=VERTEX_POINT('',#24340);
#7079=VERTEX_POINT('',#24342);
#7080=VERTEX_POINT('',#24345);
#7081=VERTEX_POINT('',#24346);
#7082=VERTEX_POINT('',#24348);
#7083=VERTEX_POINT('',#24350);
#7084=VERTEX_POINT('',#24353);
#7085=VERTEX_POINT('',#24354);
#7086=VERTEX_POINT('',#24356);
#7087=VERTEX_POINT('',#24358);
#7088=VERTEX_POINT('',#24361);
#7089=VERTEX_POINT('',#24362);
#7090=VERTEX_POINT('',#24364);
#7091=VERTEX_POINT('',#24366);
#7092=VERTEX_POINT('',#24369);
#7093=VERTEX_POINT('',#24370);
#7094=VERTEX_POINT('',#24372);
#7095=VERTEX_POINT('',#24374);
#7096=VERTEX_POINT('',#24377);
#7097=VERTEX_POINT('',#24378);
#7098=VERTEX_POINT('',#24380);
#7099=VERTEX_POINT('',#24382);
#7100=VERTEX_POINT('',#24385);
#7101=VERTEX_POINT('',#24386);
#7102=VERTEX_POINT('',#24388);
#7103=VERTEX_POINT('',#24390);
#7104=VERTEX_POINT('',#24393);
#7105=VERTEX_POINT('',#24394);
#7106=VERTEX_POINT('',#24396);
#7107=VERTEX_POINT('',#24398);
#7108=VERTEX_POINT('',#24401);
#7109=VERTEX_POINT('',#24402);
#7110=VERTEX_POINT('',#24404);
#7111=VERTEX_POINT('',#24406);
#7112=VERTEX_POINT('',#24409);
#7113=VERTEX_POINT('',#24410);
#7114=VERTEX_POINT('',#24412);
#7115=VERTEX_POINT('',#24414);
#7116=VERTEX_POINT('',#24417);
#7117=VERTEX_POINT('',#24418);
#7118=VERTEX_POINT('',#24420);
#7119=VERTEX_POINT('',#24422);
#7120=VERTEX_POINT('',#24425);
#7121=VERTEX_POINT('',#24426);
#7122=VERTEX_POINT('',#24428);
#7123=VERTEX_POINT('',#24430);
#7124=VERTEX_POINT('',#24433);
#7125=VERTEX_POINT('',#24434);
#7126=VERTEX_POINT('',#24436);
#7127=VERTEX_POINT('',#24438);
#7128=VERTEX_POINT('',#24441);
#7129=VERTEX_POINT('',#24442);
#7130=VERTEX_POINT('',#24444);
#7131=VERTEX_POINT('',#24446);
#7132=VERTEX_POINT('',#24449);
#7133=VERTEX_POINT('',#24450);
#7134=VERTEX_POINT('',#24452);
#7135=VERTEX_POINT('',#24454);
#7136=VERTEX_POINT('',#24457);
#7137=VERTEX_POINT('',#24458);
#7138=VERTEX_POINT('',#24460);
#7139=VERTEX_POINT('',#24462);
#7140=VERTEX_POINT('',#24466);
#7141=VERTEX_POINT('',#24467);
#7142=VERTEX_POINT('',#24469);
#7143=VERTEX_POINT('',#24471);
#7144=VERTEX_POINT('',#24474);
#7145=VERTEX_POINT('',#24475);
#7146=VERTEX_POINT('',#24477);
#7147=VERTEX_POINT('',#24479);
#7148=VERTEX_POINT('',#24482);
#7149=VERTEX_POINT('',#24483);
#7150=VERTEX_POINT('',#24485);
#7151=VERTEX_POINT('',#24487);
#7152=VERTEX_POINT('',#24490);
#7153=VERTEX_POINT('',#24491);
#7154=VERTEX_POINT('',#24493);
#7155=VERTEX_POINT('',#24495);
#7156=VERTEX_POINT('',#24498);
#7157=VERTEX_POINT('',#24499);
#7158=VERTEX_POINT('',#24501);
#7159=VERTEX_POINT('',#24503);
#7160=VERTEX_POINT('',#24506);
#7161=VERTEX_POINT('',#24507);
#7162=VERTEX_POINT('',#24509);
#7163=VERTEX_POINT('',#24511);
#7164=VERTEX_POINT('',#24514);
#7165=VERTEX_POINT('',#24515);
#7166=VERTEX_POINT('',#24517);
#7167=VERTEX_POINT('',#24519);
#7168=VERTEX_POINT('',#24522);
#7169=VERTEX_POINT('',#24523);
#7170=VERTEX_POINT('',#24525);
#7171=VERTEX_POINT('',#24527);
#7172=VERTEX_POINT('',#24530);
#7173=VERTEX_POINT('',#24531);
#7174=VERTEX_POINT('',#24533);
#7175=VERTEX_POINT('',#24535);
#7176=VERTEX_POINT('',#24538);
#7177=VERTEX_POINT('',#24539);
#7178=VERTEX_POINT('',#24541);
#7179=VERTEX_POINT('',#24543);
#7180=VERTEX_POINT('',#24546);
#7181=VERTEX_POINT('',#24547);
#7182=VERTEX_POINT('',#24549);
#7183=VERTEX_POINT('',#24551);
#7184=VERTEX_POINT('',#24554);
#7185=VERTEX_POINT('',#24555);
#7186=VERTEX_POINT('',#24557);
#7187=VERTEX_POINT('',#24559);
#7188=VERTEX_POINT('',#24562);
#7189=VERTEX_POINT('',#24563);
#7190=VERTEX_POINT('',#24565);
#7191=VERTEX_POINT('',#24567);
#7192=VERTEX_POINT('',#24570);
#7193=VERTEX_POINT('',#24571);
#7194=VERTEX_POINT('',#24573);
#7195=VERTEX_POINT('',#24575);
#7196=VERTEX_POINT('',#24578);
#7197=VERTEX_POINT('',#24579);
#7198=VERTEX_POINT('',#24581);
#7199=VERTEX_POINT('',#24583);
#7200=VERTEX_POINT('',#24586);
#7201=VERTEX_POINT('',#24587);
#7202=VERTEX_POINT('',#24589);
#7203=VERTEX_POINT('',#24591);
#7204=VERTEX_POINT('',#24594);
#7205=VERTEX_POINT('',#24595);
#7206=VERTEX_POINT('',#24597);
#7207=VERTEX_POINT('',#24599);
#7208=VERTEX_POINT('',#24602);
#7209=VERTEX_POINT('',#24603);
#7210=VERTEX_POINT('',#24605);
#7211=VERTEX_POINT('',#24607);
#7212=VERTEX_POINT('',#24610);
#7213=VERTEX_POINT('',#24611);
#7214=VERTEX_POINT('',#24613);
#7215=VERTEX_POINT('',#24615);
#7216=VERTEX_POINT('',#24618);
#7217=VERTEX_POINT('',#24619);
#7218=VERTEX_POINT('',#24621);
#7219=VERTEX_POINT('',#24623);
#7220=VERTEX_POINT('',#24626);
#7221=VERTEX_POINT('',#24627);
#7222=VERTEX_POINT('',#24629);
#7223=VERTEX_POINT('',#24631);
#7224=VERTEX_POINT('',#24634);
#7225=VERTEX_POINT('',#24635);
#7226=VERTEX_POINT('',#24637);
#7227=VERTEX_POINT('',#24639);
#7228=VERTEX_POINT('',#24642);
#7229=VERTEX_POINT('',#24643);
#7230=VERTEX_POINT('',#24645);
#7231=VERTEX_POINT('',#24647);
#7232=VERTEX_POINT('',#24650);
#7233=VERTEX_POINT('',#24651);
#7234=VERTEX_POINT('',#24653);
#7235=VERTEX_POINT('',#24655);
#7236=VERTEX_POINT('',#24658);
#7237=VERTEX_POINT('',#24659);
#7238=VERTEX_POINT('',#24661);
#7239=VERTEX_POINT('',#24663);
#7240=VERTEX_POINT('',#24666);
#7241=VERTEX_POINT('',#24667);
#7242=VERTEX_POINT('',#24669);
#7243=VERTEX_POINT('',#24671);
#7244=VERTEX_POINT('',#24674);
#7245=VERTEX_POINT('',#24675);
#7246=VERTEX_POINT('',#24677);
#7247=VERTEX_POINT('',#24679);
#7248=VERTEX_POINT('',#24682);
#7249=VERTEX_POINT('',#24684);
#7250=VERTEX_POINT('',#24686);
#7251=VERTEX_POINT('',#24688);
#7252=VERTEX_POINT('',#24690);
#7253=VERTEX_POINT('',#24692);
#7254=VERTEX_POINT('',#24694);
#7255=VERTEX_POINT('',#24696);
#7256=VERTEX_POINT('',#24698);
#7257=VERTEX_POINT('',#24700);
#7258=VERTEX_POINT('',#24702);
#7259=VERTEX_POINT('',#24704);
#7260=VERTEX_POINT('',#24706);
#7261=VERTEX_POINT('',#24708);
#7262=VERTEX_POINT('',#24710);
#7263=VERTEX_POINT('',#24712);
#7264=VERTEX_POINT('',#24714);
#7265=VERTEX_POINT('',#24716);
#7266=VERTEX_POINT('',#24718);
#7267=VERTEX_POINT('',#24720);
#7268=VERTEX_POINT('',#24722);
#7269=VERTEX_POINT('',#24724);
#7270=VERTEX_POINT('',#24726);
#7271=VERTEX_POINT('',#24728);
#7272=VERTEX_POINT('',#24730);
#7273=VERTEX_POINT('',#24732);
#7274=VERTEX_POINT('',#25004);
#7275=VERTEX_POINT('',#25005);
#7276=VERTEX_POINT('',#25007);
#7277=VERTEX_POINT('',#25009);
#7278=VERTEX_POINT('',#25011);
#7279=VERTEX_POINT('',#25013);
#7280=VERTEX_POINT('',#25021);
#7281=VERTEX_POINT('',#25022);
#7282=VERTEX_POINT('',#25024);
#7283=VERTEX_POINT('',#25026);
#7284=VERTEX_POINT('',#25028);
#7285=VERTEX_POINT('',#25030);
#7286=VERTEX_POINT('',#25038);
#7287=VERTEX_POINT('',#25039);
#7288=VERTEX_POINT('',#25041);
#7289=VERTEX_POINT('',#25043);
#7290=VERTEX_POINT('',#25045);
#7291=VERTEX_POINT('',#25047);
#7292=VERTEX_POINT('',#25063);
#7293=VERTEX_POINT('',#25064);
#7294=VERTEX_POINT('',#25066);
#7295=VERTEX_POINT('',#25068);
#7296=VERTEX_POINT('',#25072);
#7297=VERTEX_POINT('',#25073);
#7298=VERTEX_POINT('',#25075);
#7299=VERTEX_POINT('',#25082);
#7300=VERTEX_POINT('',#25083);
#7301=VERTEX_POINT('',#25085);
#7302=VERTEX_POINT('',#25087);
#7303=VERTEX_POINT('',#25090);
#7304=VERTEX_POINT('',#25092);
#7305=VERTEX_POINT('',#25098);
#7306=VERTEX_POINT('',#25099);
#7307=VERTEX_POINT('',#25101);
#7308=VERTEX_POINT('',#25114);
#7309=VERTEX_POINT('',#25115);
#7310=VERTEX_POINT('',#25117);
#7311=VERTEX_POINT('',#25122);
#7312=VERTEX_POINT('',#25124);
#7313=VERTEX_POINT('',#25128);
#7314=VERTEX_POINT('',#25129);
#7315=VERTEX_POINT('',#25131);
#7316=VERTEX_POINT('',#25133);
#7317=VERTEX_POINT('',#25135);
#7318=VERTEX_POINT('',#25139);
#7319=VERTEX_POINT('',#25141);
#7320=VERTEX_POINT('',#25145);
#7321=VERTEX_POINT('',#25147);
#7322=VERTEX_POINT('',#25151);
#7323=VERTEX_POINT('',#25153);
#7324=VERTEX_POINT('',#25157);
#7325=VERTEX_POINT('',#25159);
#7326=VERTEX_POINT('',#25161);
#7327=VERTEX_POINT('',#25168);
#7328=VERTEX_POINT('',#25169);
#7329=VERTEX_POINT('',#25171);
#7330=VERTEX_POINT('',#25173);
#7331=VERTEX_POINT('',#25177);
#7332=VERTEX_POINT('',#25179);
#7333=VERTEX_POINT('',#25181);
#7334=VERTEX_POINT('',#25183);
#7335=VERTEX_POINT('',#25189);
#7336=VERTEX_POINT('',#25191);
#7337=VERTEX_POINT('',#25198);
#7338=VERTEX_POINT('',#25200);
#7339=VERTEX_POINT('',#25205);
#7340=VERTEX_POINT('',#25206);
#7341=VERTEX_POINT('',#25208);
#7342=VERTEX_POINT('',#25210);
#7343=VERTEX_POINT('',#25214);
#7344=VERTEX_POINT('',#25215);
#7345=VERTEX_POINT('',#25217);
#7346=VERTEX_POINT('',#25219);
#7347=VERTEX_POINT('',#25223);
#7348=VERTEX_POINT('',#25224);
#7349=VERTEX_POINT('',#25226);
#7350=VERTEX_POINT('',#25228);
#7351=VERTEX_POINT('',#25232);
#7352=VERTEX_POINT('',#25233);
#7353=VERTEX_POINT('',#25235);
#7354=VERTEX_POINT('',#25237);
#7355=VERTEX_POINT('',#25241);
#7356=VERTEX_POINT('',#25242);
#7357=VERTEX_POINT('',#25244);
#7358=VERTEX_POINT('',#25246);
#7359=VERTEX_POINT('',#25250);
#7360=VERTEX_POINT('',#25252);
#7361=VERTEX_POINT('',#25256);
#7362=VERTEX_POINT('',#25258);
#7363=VERTEX_POINT('',#25262);
#7364=VERTEX_POINT('',#25264);
#7365=VERTEX_POINT('',#25268);
#7366=VERTEX_POINT('',#25270);
#7367=VERTEX_POINT('',#25274);
#7368=VERTEX_POINT('',#25276);
#7369=VERTEX_POINT('',#25280);
#7370=VERTEX_POINT('',#25282);
#7371=VERTEX_POINT('',#25286);
#7372=VERTEX_POINT('',#25287);
#7373=VERTEX_POINT('',#25289);
#7374=VERTEX_POINT('',#25291);
#7375=VERTEX_POINT('',#25295);
#7376=VERTEX_POINT('',#25296);
#7377=VERTEX_POINT('',#25298);
#7378=VERTEX_POINT('',#25300);
#7379=VERTEX_POINT('',#25304);
#7380=VERTEX_POINT('',#25309);
#7381=VERTEX_POINT('',#25311);
#7382=VERTEX_POINT('',#25321);
#7383=VERTEX_POINT('',#25323);
#7384=VERTEX_POINT('',#25327);
#7385=VERTEX_POINT('',#25334);
#7386=VERTEX_POINT('',#25339);
#7387=VERTEX_POINT('',#25343);
#7388=VERTEX_POINT('',#25344);
#7389=VERTEX_POINT('',#25346);
#7390=VERTEX_POINT('',#25348);
#7391=VERTEX_POINT('',#25352);
#7392=VERTEX_POINT('',#25353);
#7393=VERTEX_POINT('',#25355);
#7394=VERTEX_POINT('',#25357);
#7395=VERTEX_POINT('',#25361);
#7396=VERTEX_POINT('',#25363);
#7397=VERTEX_POINT('',#25368);
#7398=VERTEX_POINT('',#25371);
#7399=VERTEX_POINT('',#25390);
#7400=VERTEX_POINT('',#25394);
#7401=VERTEX_POINT('',#25398);
#7402=VERTEX_POINT('',#25399);
#7403=VERTEX_POINT('',#25401);
#7404=VERTEX_POINT('',#25403);
#7405=VERTEX_POINT('',#25407);
#7406=VERTEX_POINT('',#25410);
#7407=VERTEX_POINT('',#25416);
#7408=VERTEX_POINT('',#25420);
#7409=VERTEX_POINT('',#25421);
#7410=VERTEX_POINT('',#25423);
#7411=VERTEX_POINT('',#25425);
#7412=VERTEX_POINT('',#25429);
#7413=VERTEX_POINT('',#25432);
#7414=VERTEX_POINT('',#25436);
#7415=VERTEX_POINT('',#25438);
#7416=VERTEX_POINT('',#25443);
#7417=VERTEX_POINT('',#25444);
#7418=VERTEX_POINT('',#25446);
#7419=VERTEX_POINT('',#25448);
#7420=VERTEX_POINT('',#25452);
#7421=VERTEX_POINT('',#25453);
#7422=VERTEX_POINT('',#25458);
#7423=VERTEX_POINT('',#25459);
#7424=VERTEX_POINT('',#25467);
#7425=VERTEX_POINT('',#25468);
#7426=VERTEX_POINT('',#25470);
#7427=VERTEX_POINT('',#25472);
#7428=VERTEX_POINT('',#25476);
#7429=VERTEX_POINT('',#25477);
#7430=VERTEX_POINT('',#25482);
#7431=VERTEX_POINT('',#25483);
#7432=VERTEX_POINT('',#25491);
#7433=VERTEX_POINT('',#25492);
#7434=VERTEX_POINT('',#25494);
#7435=VERTEX_POINT('',#25496);
#7436=VERTEX_POINT('',#25498);
#7437=VERTEX_POINT('',#25503);
#7438=VERTEX_POINT('',#25507);
#7439=VERTEX_POINT('',#25511);
#7440=VERTEX_POINT('',#25513);
#7441=VERTEX_POINT('',#25521);
#7442=VERTEX_POINT('',#25527);
#7443=VERTEX_POINT('',#25542);
#7444=VERTEX_POINT('',#25544);
#7445=VERTEX_POINT('',#25560);
#7446=VERTEX_POINT('',#25561);
#7447=VERTEX_POINT('',#25563);
#7448=VERTEX_POINT('',#25567);
#7449=VERTEX_POINT('',#25568);
#7450=VERTEX_POINT('',#25570);
#7451=VERTEX_POINT('',#25574);
#7452=VERTEX_POINT('',#25575);
#7453=VERTEX_POINT('',#25577);
#7454=VERTEX_POINT('',#25579);
#7455=VERTEX_POINT('',#25594);
#7456=VERTEX_POINT('',#25595);
#7457=VERTEX_POINT('',#25597);
#7458=VERTEX_POINT('',#25601);
#7459=VERTEX_POINT('',#25602);
#7460=VERTEX_POINT('',#25604);
#7461=VERTEX_POINT('',#25606);
#7462=VERTEX_POINT('',#25621);
#7463=VERTEX_POINT('',#25622);
#7464=VERTEX_POINT('',#25624);
#7465=VERTEX_POINT('',#25628);
#7466=VERTEX_POINT('',#25629);
#7467=VERTEX_POINT('',#25631);
#7468=VERTEX_POINT('',#25633);
#7469=VERTEX_POINT('',#25648);
#7470=VERTEX_POINT('',#25649);
#7471=VERTEX_POINT('',#25651);
#7472=VERTEX_POINT('',#25664);
#7473=VERTEX_POINT('',#25668);
#7474=VERTEX_POINT('',#25669);
#7475=VERTEX_POINT('',#25671);
#7476=VERTEX_POINT('',#25675);
#7477=VERTEX_POINT('',#25676);
#7478=VERTEX_POINT('',#25678);
#7479=VERTEX_POINT('',#25682);
#7480=VERTEX_POINT('',#25684);
#7481=VERTEX_POINT('',#25688);
#7482=VERTEX_POINT('',#25689);
#7483=VERTEX_POINT('',#25692);
#7484=VERTEX_POINT('',#25696);
#7485=VERTEX_POINT('',#25698);
#7486=VERTEX_POINT('',#25700);
#7487=VERTEX_POINT('',#25704);
#7488=VERTEX_POINT('',#25706);
#7489=VERTEX_POINT('',#25710);
#7490=VERTEX_POINT('',#25712);
#7491=VERTEX_POINT('',#25714);
#7492=VERTEX_POINT('',#25718);
#7493=VERTEX_POINT('',#25720);
#7494=VERTEX_POINT('',#25724);
#7495=VERTEX_POINT('',#25726);
#7496=VERTEX_POINT('',#25730);
#7497=VERTEX_POINT('',#25732);
#7498=VERTEX_POINT('',#25736);
#7499=VERTEX_POINT('',#25738);
#7500=VERTEX_POINT('',#25744);
#7501=VERTEX_POINT('',#25746);
#7502=VERTEX_POINT('',#25748);
#7503=VERTEX_POINT('',#25761);
#7504=VERTEX_POINT('',#25768);
#7505=VERTEX_POINT('',#25777);
#7506=VERTEX_POINT('',#25784);
#7507=VERTEX_POINT('',#25786);
#7508=VERTEX_POINT('',#25793);
#7509=VERTEX_POINT('',#25806);
#7510=VERTEX_POINT('',#25808);
#7511=VERTEX_POINT('',#25821);
#7512=VERTEX_POINT('',#25828);
#7513=VERTEX_POINT('',#25836);
#7514=VERTEX_POINT('',#25838);
#7515=VERTEX_POINT('',#25851);
#7516=VERTEX_POINT('',#25858);
#7517=VERTEX_POINT('',#25860);
#7518=VERTEX_POINT('',#25867);
#7519=VERTEX_POINT('',#25881);
#7520=VERTEX_POINT('',#25888);
#7521=VERTEX_POINT('',#25890);
#7522=VERTEX_POINT('',#25897);
#7523=VERTEX_POINT('',#25912);
#7524=VERTEX_POINT('',#25913);
#7525=VERTEX_POINT('',#25937);
#7526=VERTEX_POINT('',#25960);
#7527=VERTEX_POINT('',#25984);
#7528=VERTEX_POINT('',#26007);
#7529=VERTEX_POINT('',#26009);
#7530=VERTEX_POINT('',#26012);
#7531=VERTEX_POINT('',#26036);
#7532=VERTEX_POINT('',#26059);
#7533=VERTEX_POINT('',#26083);
#7534=VERTEX_POINT('',#26106);
#7535=VERTEX_POINT('',#26159);
#7536=VERTEX_POINT('',#26167);
#7537=VERTEX_POINT('',#26168);
#7538=VERTEX_POINT('',#26171);
#7539=VERTEX_POINT('',#26175);
#7540=VERTEX_POINT('',#26177);
#7541=VERTEX_POINT('',#26181);
#7542=VERTEX_POINT('',#26182);
#7543=VERTEX_POINT('',#26185);
#7544=VERTEX_POINT('',#26189);
#7545=VERTEX_POINT('',#26191);
#7546=VERTEX_POINT('',#26198);
#7547=VERTEX_POINT('',#26202);
#7548=VERTEX_POINT('',#26204);
#7549=VERTEX_POINT('',#26219);
#7550=VERTEX_POINT('',#26223);
#7551=VERTEX_POINT('',#26224);
#7552=VERTEX_POINT('',#26242);
#7553=VERTEX_POINT('',#26249);
#7554=VERTEX_POINT('',#26253);
#7555=VERTEX_POINT('',#26254);
#7556=VERTEX_POINT('',#26274);
#7557=VERTEX_POINT('',#26275);
#7558=VERTEX_POINT('',#26298);
#7559=VERTEX_POINT('',#26300);
#7560=VERTEX_POINT('',#26302);
#7561=VERTEX_POINT('',#26322);
#7562=VERTEX_POINT('',#26326);
#7563=VERTEX_POINT('',#26327);
#7564=VERTEX_POINT('',#26330);
#7565=VERTEX_POINT('',#26334);
#7566=VERTEX_POINT('',#26335);
#7567=VERTEX_POINT('',#26338);
#7568=VERTEX_POINT('',#26357);
#7569=VERTEX_POINT('',#26358);
#7570=VERTEX_POINT('',#26376);
#7571=VERTEX_POINT('',#26380);
#7572=VERTEX_POINT('',#26382);
#7573=VERTEX_POINT('',#26402);
#7574=VERTEX_POINT('',#26406);
#7575=VERTEX_POINT('',#26416);
#7576=VERTEX_POINT('',#26417);
#7577=VERTEX_POINT('',#26419);
#7578=VERTEX_POINT('',#26424);
#7579=VERTEX_POINT('',#26428);
#7580=VERTEX_POINT('',#26437);
#7581=VERTEX_POINT('',#26439);
#7582=VERTEX_POINT('',#26454);
#7583=VERTEX_POINT('',#26461);
#7584=VERTEX_POINT('',#26462);
#7585=VERTEX_POINT('',#26480);
#7586=VERTEX_POINT('',#26484);
#7587=VERTEX_POINT('',#26485);
#7588=VERTEX_POINT('',#26490);
#7589=VERTEX_POINT('',#26491);
#7590=VERTEX_POINT('',#26511);
#7591=VERTEX_POINT('',#26512);
#7592=VERTEX_POINT('',#26532);
#7593=VERTEX_POINT('',#26539);
#7594=VERTEX_POINT('',#26541);
#7595=VERTEX_POINT('',#26543);
#7596=VERTEX_POINT('',#26563);
#7597=VERTEX_POINT('',#26565);
#7598=VERTEX_POINT('',#26570);
#7599=VERTEX_POINT('',#26574);
#7600=VERTEX_POINT('',#26575);
#7601=VERTEX_POINT('',#26578);
#7602=VERTEX_POINT('',#26597);
#7603=VERTEX_POINT('',#26598);
#7604=VERTEX_POINT('',#26616);
#7605=VERTEX_POINT('',#26620);
#7606=VERTEX_POINT('',#26622);
#7607=VERTEX_POINT('',#26641);
#7608=VERTEX_POINT('',#26644);
#7609=VERTEX_POINT('',#26653);
#7610=VERTEX_POINT('',#26654);
#7611=VERTEX_POINT('',#26659);
#7612=VERTEX_POINT('',#26664);
#7613=VERTEX_POINT('',#26668);
#7614=VERTEX_POINT('',#26675);
#7615=VERTEX_POINT('',#26679);
#7616=VERTEX_POINT('',#26681);
#7617=VERTEX_POINT('',#26696);
#7618=VERTEX_POINT('',#26703);
#7619=VERTEX_POINT('',#26704);
#7620=VERTEX_POINT('',#26722);
#7621=VERTEX_POINT('',#26727);
#7622=VERTEX_POINT('',#26731);
#7623=VERTEX_POINT('',#26735);
#7624=VERTEX_POINT('',#26736);
#7625=VERTEX_POINT('',#26756);
#7626=VERTEX_POINT('',#26757);
#7627=VERTEX_POINT('',#26781);
#7628=VERTEX_POINT('',#26785);
#7629=VERTEX_POINT('',#26790);
#7630=VERTEX_POINT('',#26792);
#7631=VERTEX_POINT('',#26821);
#7632=VERTEX_POINT('',#26824);
#7633=VERTEX_POINT('',#26843);
#7634=VERTEX_POINT('',#26844);
#7635=VERTEX_POINT('',#26846);
#7636=VERTEX_POINT('',#26848);
#7637=VERTEX_POINT('',#26852);
#7638=VERTEX_POINT('',#26853);
#7639=VERTEX_POINT('',#26855);
#7640=VERTEX_POINT('',#26857);
#7641=VERTEX_POINT('',#26861);
#7642=VERTEX_POINT('',#26862);
#7643=VERTEX_POINT('',#26864);
#7644=VERTEX_POINT('',#26866);
#7645=VERTEX_POINT('',#26870);
#7646=VERTEX_POINT('',#26871);
#7647=VERTEX_POINT('',#26873);
#7648=VERTEX_POINT('',#26875);
#7649=VERTEX_POINT('',#26879);
#7650=VERTEX_POINT('',#26880);
#7651=VERTEX_POINT('',#26882);
#7652=VERTEX_POINT('',#26884);
#7653=VERTEX_POINT('',#26888);
#7654=VERTEX_POINT('',#26889);
#7655=VERTEX_POINT('',#26891);
#7656=VERTEX_POINT('',#26893);
#7657=VERTEX_POINT('',#26897);
#7658=VERTEX_POINT('',#26898);
#7659=VERTEX_POINT('',#26901);
#7660=VERTEX_POINT('',#26905);
#7661=VERTEX_POINT('',#26906);
#7662=VERTEX_POINT('',#26909);
#7663=VERTEX_POINT('',#26913);
#7664=VERTEX_POINT('',#26914);
#7665=VERTEX_POINT('',#26917);
#7666=VERTEX_POINT('',#26921);
#7667=VERTEX_POINT('',#26922);
#7668=VERTEX_POINT('',#26925);
#7669=VERTEX_POINT('',#26929);
#7670=VERTEX_POINT('',#26930);
#7671=VERTEX_POINT('',#26933);
#7672=VERTEX_POINT('',#26937);
#7673=VERTEX_POINT('',#26938);
#7674=VERTEX_POINT('',#26941);
#7675=VERTEX_POINT('',#26945);
#7676=VERTEX_POINT('',#26946);
#7677=VERTEX_POINT('',#26949);
#7678=VERTEX_POINT('',#26953);
#7679=VERTEX_POINT('',#26954);
#7680=VERTEX_POINT('',#26957);
#7681=VERTEX_POINT('',#26961);
#7682=VERTEX_POINT('',#26962);
#7683=VERTEX_POINT('',#26965);
#7684=VERTEX_POINT('',#26969);
#7685=VERTEX_POINT('',#26970);
#7686=VERTEX_POINT('',#26973);
#7687=VERTEX_POINT('',#26977);
#7688=VERTEX_POINT('',#26978);
#7689=VERTEX_POINT('',#26981);
#7690=VERTEX_POINT('',#26985);
#7691=VERTEX_POINT('',#26986);
#7692=VERTEX_POINT('',#26989);
#7693=VERTEX_POINT('',#26993);
#7694=VERTEX_POINT('',#26994);
#7695=VERTEX_POINT('',#26997);
#7696=VERTEX_POINT('',#27001);
#7697=VERTEX_POINT('',#27002);
#7698=VERTEX_POINT('',#27004);
#7699=VERTEX_POINT('',#27006);
#7700=VERTEX_POINT('',#27010);
#7701=VERTEX_POINT('',#27011);
#7702=VERTEX_POINT('',#27013);
#7703=VERTEX_POINT('',#27015);
#7704=VERTEX_POINT('',#27017);
#7705=VERTEX_POINT('',#27019);
#7706=VERTEX_POINT('',#27021);
#7707=VERTEX_POINT('',#27023);
#7708=VERTEX_POINT('',#27025);
#7709=VERTEX_POINT('',#27029);
#7710=VERTEX_POINT('',#27030);
#7711=VERTEX_POINT('',#27032);
#7712=VERTEX_POINT('',#27034);
#7713=VERTEX_POINT('',#27038);
#7714=VERTEX_POINT('',#27039);
#7715=VERTEX_POINT('',#27042);
#7716=VERTEX_POINT('',#27046);
#7717=VERTEX_POINT('',#27050);
#7718=VERTEX_POINT('',#27052);
#7719=VERTEX_POINT('',#27056);
#7720=VERTEX_POINT('',#27058);
#7721=VERTEX_POINT('',#27063);
#7722=VERTEX_POINT('',#27065);
#7723=VERTEX_POINT('',#27069);
#7724=VERTEX_POINT('',#27070);
#7725=VERTEX_POINT('',#27072);
#7726=VERTEX_POINT('',#27074);
#7727=VERTEX_POINT('',#27079);
#7728=VERTEX_POINT('',#27081);
#7729=VERTEX_POINT('',#27085);
#7730=VERTEX_POINT('',#27087);
#7731=VERTEX_POINT('',#27089);
#7732=VERTEX_POINT('',#27092);
#7733=VERTEX_POINT('',#27113);
#7734=VERTEX_POINT('',#27117);
#7735=VERTEX_POINT('',#27119);
#7736=VERTEX_POINT('',#27123);
#7737=VERTEX_POINT('',#27127);
#7738=VERTEX_POINT('',#27131);
#7739=VERTEX_POINT('',#27135);
#7740=VERTEX_POINT('',#27137);
#7741=VERTEX_POINT('',#27141);
#7742=VERTEX_POINT('',#27143);
#7743=VERTEX_POINT('',#27147);
#7744=VERTEX_POINT('',#27151);
#7745=VERTEX_POINT('',#27155);
#7746=VERTEX_POINT('',#27159);
#7747=VERTEX_POINT('',#27163);
#7748=VERTEX_POINT('',#27167);
#7749=VERTEX_POINT('',#27171);
#7750=VERTEX_POINT('',#27175);
#7751=VERTEX_POINT('',#27179);
#7752=VERTEX_POINT('',#27183);
#7753=VERTEX_POINT('',#27184);
#7754=VERTEX_POINT('',#27186);
#7755=VERTEX_POINT('',#27188);
#7756=VERTEX_POINT('',#27192);
#7757=VERTEX_POINT('',#27194);
#7758=VERTEX_POINT('',#27201);
#7759=VERTEX_POINT('',#27203);
#7760=VERTEX_POINT('',#27207);
#7761=VERTEX_POINT('',#27209);
#7762=VERTEX_POINT('',#27216);
#7763=VERTEX_POINT('',#27218);
#7764=VERTEX_POINT('',#27222);
#7765=VERTEX_POINT('',#27224);
#7766=VERTEX_POINT('',#27228);
#7767=VERTEX_POINT('',#27230);
#7768=VERTEX_POINT('',#27234);
#7769=VERTEX_POINT('',#27236);
#7770=VERTEX_POINT('',#27240);
#7771=VERTEX_POINT('',#27242);
#7772=VERTEX_POINT('',#27247);
#7773=VERTEX_POINT('',#27251);
#7774=VERTEX_POINT('',#27255);
#7775=VERTEX_POINT('',#27259);
#7776=VERTEX_POINT('',#27261);
#7777=VERTEX_POINT('',#27263);
#7778=VERTEX_POINT('',#27266);
#7779=VERTEX_POINT('',#27270);
#7780=VERTEX_POINT('',#27272);
#7781=VERTEX_POINT('',#27276);
#7782=VERTEX_POINT('',#27278);
#7783=VERTEX_POINT('',#27298);
#7784=VERTEX_POINT('',#27299);
#7785=VERTEX_POINT('',#27301);
#7786=VERTEX_POINT('',#27303);
#7787=VERTEX_POINT('',#27307);
#7788=VERTEX_POINT('',#27308);
#7789=VERTEX_POINT('',#27310);
#7790=VERTEX_POINT('',#27312);
#7791=VERTEX_POINT('',#27316);
#7792=VERTEX_POINT('',#27347);
#7793=VERTEX_POINT('',#27349);
#7794=VERTEX_POINT('',#27351);
#7795=VERTEX_POINT('',#27381);
#7796=VERTEX_POINT('',#27383);
#7797=VERTEX_POINT('',#27385);
#7798=VERTEX_POINT('',#27390);
#7799=VERTEX_POINT('',#27395);
#7800=VERTEX_POINT('',#27401);
#7801=VERTEX_POINT('',#27402);
#7802=VERTEX_POINT('',#27404);
#7803=VERTEX_POINT('',#27406);
#7804=VERTEX_POINT('',#27410);
#7805=VERTEX_POINT('',#27411);
#7806=VERTEX_POINT('',#27416);
#7807=VERTEX_POINT('',#27427);
#7808=VERTEX_POINT('',#27428);
#7809=VERTEX_POINT('',#27430);
#7810=VERTEX_POINT('',#27432);
#7811=VERTEX_POINT('',#27436);
#7812=VERTEX_POINT('',#27437);
#7813=VERTEX_POINT('',#27439);
#7814=VERTEX_POINT('',#27441);
#7815=VERTEX_POINT('',#27445);
#7816=VERTEX_POINT('',#27446);
#7817=VERTEX_POINT('',#27448);
#7818=VERTEX_POINT('',#27450);
#7819=VERTEX_POINT('',#27454);
#7820=VERTEX_POINT('',#27455);
#7821=VERTEX_POINT('',#27457);
#7822=VERTEX_POINT('',#27459);
#7823=VERTEX_POINT('',#27463);
#7824=VERTEX_POINT('',#27464);
#7825=VERTEX_POINT('',#27466);
#7826=VERTEX_POINT('',#27468);
#7827=VERTEX_POINT('',#27472);
#7828=VERTEX_POINT('',#27473);
#7829=VERTEX_POINT('',#27475);
#7830=VERTEX_POINT('',#27477);
#7831=VERTEX_POINT('',#27481);
#7832=VERTEX_POINT('',#27483);
#7833=VERTEX_POINT('',#27490);
#7834=VERTEX_POINT('',#27492);
#7835=VERTEX_POINT('',#27499);
#7836=VERTEX_POINT('',#27502);
#7837=VERTEX_POINT('',#27504);
#7838=VERTEX_POINT('',#27506);
#7839=VERTEX_POINT('',#27508);
#7840=VERTEX_POINT('',#27510);
#7841=VERTEX_POINT('',#27512);
#7842=VERTEX_POINT('',#27516);
#7843=VERTEX_POINT('',#27519);
#7844=VERTEX_POINT('',#27521);
#7845=VERTEX_POINT('',#27523);
#7846=VERTEX_POINT('',#27525);
#7847=VERTEX_POINT('',#27527);
#7848=VERTEX_POINT('',#27529);
#7849=VERTEX_POINT('',#27556);
#7850=VERTEX_POINT('',#27557);
#7851=VERTEX_POINT('',#27559);
#7852=VERTEX_POINT('',#27561);
#7853=VERTEX_POINT('',#27582);
#7854=VERTEX_POINT('',#27583);
#7855=VERTEX_POINT('',#27658);
#7856=VERTEX_POINT('',#27659);
#7857=VERTEX_POINT('',#27734);
#7858=VERTEX_POINT('',#27735);
#7859=VERTEX_POINT('',#27812);
#7860=VERTEX_POINT('',#27813);
#7861=VERTEX_POINT('',#27888);
#7862=VERTEX_POINT('',#27889);
#7863=VERTEX_POINT('',#27964);
#7864=VERTEX_POINT('',#27965);
#7865=VERTEX_POINT('',#28040);
#7866=VERTEX_POINT('',#28041);
#7867=VERTEX_POINT('',#28116);
#7868=VERTEX_POINT('',#28117);
#7869=VERTEX_POINT('',#28194);
#7870=VERTEX_POINT('',#28195);
#7871=VERTEX_POINT('',#28270);
#7872=VERTEX_POINT('',#28271);
#7873=VERTEX_POINT('',#28346);
#7874=VERTEX_POINT('',#28347);
#7875=VERTEX_POINT('',#28424);
#7876=VERTEX_POINT('',#28425);
#7877=VERTEX_POINT('',#28500);
#7878=VERTEX_POINT('',#28501);
#7879=VERTEX_POINT('',#28576);
#7880=VERTEX_POINT('',#28577);
#7881=VERTEX_POINT('',#28652);
#7882=VERTEX_POINT('',#28653);
#7883=VERTEX_POINT('',#28730);
#7884=VERTEX_POINT('',#28731);
#7885=VERTEX_POINT('',#28806);
#7886=VERTEX_POINT('',#28807);
#7887=VERTEX_POINT('',#28882);
#7888=VERTEX_POINT('',#28883);
#7889=VERTEX_POINT('',#28885);
#7890=VERTEX_POINT('',#28918);
#7891=VERTEX_POINT('',#28955);
#7892=VERTEX_POINT('',#28956);
#7893=VERTEX_POINT('',#28959);
#7894=VERTEX_POINT('',#28961);
#7895=VERTEX_POINT('',#28971);
#7896=VERTEX_POINT('',#28972);
#7897=VERTEX_POINT('',#28974);
#7898=VERTEX_POINT('',#28982);
#7899=VERTEX_POINT('',#28992);
#7900=VERTEX_POINT('',#28993);
#7901=VERTEX_POINT('',#29022);
#7902=VERTEX_POINT('',#29023);
#7903=VERTEX_POINT('',#29052);
#7904=VERTEX_POINT('',#29053);
#7905=VERTEX_POINT('',#29082);
#7906=VERTEX_POINT('',#29083);
#7907=VERTEX_POINT('',#29112);
#7908=VERTEX_POINT('',#29113);
#7909=VERTEX_POINT('',#29142);
#7910=VERTEX_POINT('',#29143);
#7911=VERTEX_POINT('',#29172);
#7912=VERTEX_POINT('',#29173);
#7913=VERTEX_POINT('',#29202);
#7914=VERTEX_POINT('',#29203);
#7915=VERTEX_POINT('',#29232);
#7916=VERTEX_POINT('',#29233);
#7917=VERTEX_POINT('',#29262);
#7918=VERTEX_POINT('',#29263);
#7919=VERTEX_POINT('',#29292);
#7920=VERTEX_POINT('',#29293);
#7921=VERTEX_POINT('',#29322);
#7922=VERTEX_POINT('',#29323);
#7923=VERTEX_POINT('',#29352);
#7924=VERTEX_POINT('',#29353);
#7925=VERTEX_POINT('',#29382);
#7926=VERTEX_POINT('',#29383);
#7927=VERTEX_POINT('',#29412);
#7928=VERTEX_POINT('',#29413);
#7929=VERTEX_POINT('',#29442);
#7930=VERTEX_POINT('',#29443);
#7931=VERTEX_POINT('',#29472);
#7932=VERTEX_POINT('',#29473);
#7933=VERTEX_POINT('',#29502);
#7934=VERTEX_POINT('',#29503);
#7935=VERTEX_POINT('',#29532);
#7936=VERTEX_POINT('',#29533);
#7937=VERTEX_POINT('',#29535);
#7938=VERTEX_POINT('',#29543);
#7939=VERTEX_POINT('',#29553);
#7940=VERTEX_POINT('',#29554);
#7941=VERTEX_POINT('',#29556);
#7942=VERTEX_POINT('',#29589);
#7943=VERTEX_POINT('',#29620);
#7944=VERTEX_POINT('',#29621);
#7945=VERTEX_POINT('',#29696);
#7946=VERTEX_POINT('',#29697);
#7947=VERTEX_POINT('',#29772);
#7948=VERTEX_POINT('',#29773);
#7949=VERTEX_POINT('',#29775);
#7950=VERTEX_POINT('',#29785);
#7951=VERTEX_POINT('',#29797);
#7952=VERTEX_POINT('',#29798);
#7953=VERTEX_POINT('',#29835);
#7954=VERTEX_POINT('',#29836);
#7955=VERTEX_POINT('',#29873);
#7956=VERTEX_POINT('',#29874);
#7957=VERTEX_POINT('',#29911);
#7958=VERTEX_POINT('',#29912);
#7959=VERTEX_POINT('',#29949);
#7960=VERTEX_POINT('',#29950);
#7961=VERTEX_POINT('',#29987);
#7962=VERTEX_POINT('',#29988);
#7963=VERTEX_POINT('',#30025);
#7964=VERTEX_POINT('',#30026);
#7965=VERTEX_POINT('',#30063);
#7966=VERTEX_POINT('',#30064);
#7967=VERTEX_POINT('',#30066);
#7968=VERTEX_POINT('',#30077);
#7969=VERTEX_POINT('',#30110);
#7970=VERTEX_POINT('',#30111);
#7971=VERTEX_POINT('',#30188);
#7972=VERTEX_POINT('',#30189);
#7973=VERTEX_POINT('',#30264);
#7974=VERTEX_POINT('',#30265);
#7975=VERTEX_POINT('',#30267);
#7976=VERTEX_POINT('',#30294);
#7977=VERTEX_POINT('',#30396);
#7978=VERTEX_POINT('',#30397);
#7979=VERTEX_POINT('',#30399);
#7980=VERTEX_POINT('',#30401);
#7981=VERTEX_POINT('',#30405);
#7982=VERTEX_POINT('',#30406);
#7983=VERTEX_POINT('',#30413);
#7984=VERTEX_POINT('',#30417);
#7985=VERTEX_POINT('',#30421);
#7986=VERTEX_POINT('',#30425);
#7987=VERTEX_POINT('',#30429);
#7988=VERTEX_POINT('',#30430);
#7989=VERTEX_POINT('',#30432);
#7990=VERTEX_POINT('',#30434);
#7991=VERTEX_POINT('',#30438);
#7992=VERTEX_POINT('',#30439);
#7993=VERTEX_POINT('',#30443);
#7994=VERTEX_POINT('',#30448);
#7995=VERTEX_POINT('',#30454);
#7996=VERTEX_POINT('',#30458);
#7997=VERTEX_POINT('',#30462);
#7998=VERTEX_POINT('',#30463);
#7999=VERTEX_POINT('',#30465);
#8000=VERTEX_POINT('',#30467);
#8001=VERTEX_POINT('',#30471);
#8002=VERTEX_POINT('',#30472);
#8003=VERTEX_POINT('',#30476);
#8004=VERTEX_POINT('',#30481);
#8005=VERTEX_POINT('',#30487);
#8006=VERTEX_POINT('',#30491);
#8007=VERTEX_POINT('',#30495);
#8008=VERTEX_POINT('',#30496);
#8009=VERTEX_POINT('',#30498);
#8010=VERTEX_POINT('',#30500);
#8011=VERTEX_POINT('',#30502);
#8012=VERTEX_POINT('',#30506);
#8013=VERTEX_POINT('',#30507);
#8014=VERTEX_POINT('',#30511);
#8015=VERTEX_POINT('',#30516);
#8016=VERTEX_POINT('',#30517);
#8017=VERTEX_POINT('',#30526);
#8018=VERTEX_POINT('',#30530);
#8019=VERTEX_POINT('',#30539);
#8020=VERTEX_POINT('',#30569);
#8021=VERTEX_POINT('',#30571);
#8022=VERTEX_POINT('',#30575);
#8023=VERTEX_POINT('',#30850);
#8024=VERTEX_POINT('',#30861);
#8025=VERTEX_POINT('',#30863);
#8026=VERTEX_POINT('',#31161);
#8027=VERTEX_POINT('',#31183);
#8028=VERTEX_POINT('',#31197);
#8029=VERTEX_POINT('',#31200);
#8030=VERTEX_POINT('',#31202);
#8031=VERTEX_POINT('',#31213);
#8032=VERTEX_POINT('',#31215);
#8033=VERTEX_POINT('',#31217);
#8034=VERTEX_POINT('',#31221);
#8035=VERTEX_POINT('',#31223);
#8036=VERTEX_POINT('',#31227);
#8037=VERTEX_POINT('',#31229);
#8038=VERTEX_POINT('',#31234);
#8039=VERTEX_POINT('',#31237);
#8040=VERTEX_POINT('',#31238);
#8041=VERTEX_POINT('',#31240);
#8042=VERTEX_POINT('',#31242);
#8043=VERTEX_POINT('',#31244);
#8044=VERTEX_POINT('',#31246);
#8045=VERTEX_POINT('',#31249);
#8046=VERTEX_POINT('',#31251);
#8047=VERTEX_POINT('',#31253);
#8048=VERTEX_POINT('',#31259);
#8049=VERTEX_POINT('',#31269);
#8050=VERTEX_POINT('',#31274);
#8051=VERTEX_POINT('',#31276);
#8052=VERTEX_POINT('',#31281);
#8053=VERTEX_POINT('',#31283);
#8054=VERTEX_POINT('',#31288);
#8055=VERTEX_POINT('',#31290);
#8056=VERTEX_POINT('',#31295);
#8057=VERTEX_POINT('',#31299);
#8058=VERTEX_POINT('',#31300);
#8059=VERTEX_POINT('',#31302);
#8060=VERTEX_POINT('',#31304);
#8061=VERTEX_POINT('',#31308);
#8062=VERTEX_POINT('',#31310);
#8063=VERTEX_POINT('',#31314);
#8064=VERTEX_POINT('',#31316);
#8065=VERTEX_POINT('',#31320);
#8066=VERTEX_POINT('',#31322);
#8067=VERTEX_POINT('',#31326);
#8068=VERTEX_POINT('',#31328);
#8069=VERTEX_POINT('',#31332);
#8070=VERTEX_POINT('',#31334);
#8071=VERTEX_POINT('',#31338);
#8072=VERTEX_POINT('',#31340);
#8073=VERTEX_POINT('',#31344);
#8074=VERTEX_POINT('',#31346);
#8075=VERTEX_POINT('',#31350);
#8076=VERTEX_POINT('',#31352);
#8077=VERTEX_POINT('',#31356);
#8078=VERTEX_POINT('',#31358);
#8079=VERTEX_POINT('',#31362);
#8080=VERTEX_POINT('',#31364);
#8081=VERTEX_POINT('',#31368);
#8082=VERTEX_POINT('',#31370);
#8083=VERTEX_POINT('',#31374);
#8084=VERTEX_POINT('',#31376);
#8085=VERTEX_POINT('',#31380);
#8086=VERTEX_POINT('',#31382);
#8087=VERTEX_POINT('',#31386);
#8088=VERTEX_POINT('',#31388);
#8089=VERTEX_POINT('',#31392);
#8090=VERTEX_POINT('',#31394);
#8091=VERTEX_POINT('',#31398);
#8092=VERTEX_POINT('',#31400);
#8093=VERTEX_POINT('',#31404);
#8094=VERTEX_POINT('',#31406);
#8095=VERTEX_POINT('',#31410);
#8096=VERTEX_POINT('',#31412);
#8097=VERTEX_POINT('',#31416);
#8098=VERTEX_POINT('',#31418);
#8099=VERTEX_POINT('',#31422);
#8100=VERTEX_POINT('',#31424);
#8101=VERTEX_POINT('',#31428);
#8102=VERTEX_POINT('',#31430);
#8103=VERTEX_POINT('',#31434);
#8104=VERTEX_POINT('',#31436);
#8105=VERTEX_POINT('',#31440);
#8106=VERTEX_POINT('',#31442);
#8107=VERTEX_POINT('',#31446);
#8108=VERTEX_POINT('',#31448);
#8109=VERTEX_POINT('',#31452);
#8110=VERTEX_POINT('',#31454);
#8111=VERTEX_POINT('',#31458);
#8112=VERTEX_POINT('',#31460);
#8113=VERTEX_POINT('',#31464);
#8114=VERTEX_POINT('',#31466);
#8115=VERTEX_POINT('',#31470);
#8116=VERTEX_POINT('',#31472);
#8117=VERTEX_POINT('',#31476);
#8118=VERTEX_POINT('',#31478);
#8119=VERTEX_POINT('',#31482);
#8120=VERTEX_POINT('',#31484);
#8121=VERTEX_POINT('',#31488);
#8122=VERTEX_POINT('',#31490);
#8123=VERTEX_POINT('',#31494);
#8124=VERTEX_POINT('',#31496);
#8125=VERTEX_POINT('',#31500);
#8126=VERTEX_POINT('',#31502);
#8127=VERTEX_POINT('',#31506);
#8128=VERTEX_POINT('',#31508);
#8129=VERTEX_POINT('',#31512);
#8130=VERTEX_POINT('',#31514);
#8131=VERTEX_POINT('',#31518);
#8132=VERTEX_POINT('',#31520);
#8133=VERTEX_POINT('',#31524);
#8134=VERTEX_POINT('',#31526);
#8135=VERTEX_POINT('',#31530);
#8136=VERTEX_POINT('',#31532);
#8137=VERTEX_POINT('',#31536);
#8138=VERTEX_POINT('',#31538);
#8139=VERTEX_POINT('',#31542);
#8140=VERTEX_POINT('',#31544);
#8141=VERTEX_POINT('',#31548);
#8142=VERTEX_POINT('',#31550);
#8143=VERTEX_POINT('',#31554);
#8144=VERTEX_POINT('',#31556);
#8145=VERTEX_POINT('',#31560);
#8146=VERTEX_POINT('',#31562);
#8147=VERTEX_POINT('',#31566);
#8148=VERTEX_POINT('',#31568);
#8149=VERTEX_POINT('',#31572);
#8150=VERTEX_POINT('',#31574);
#8151=VERTEX_POINT('',#31578);
#8152=VERTEX_POINT('',#31580);
#8153=VERTEX_POINT('',#31584);
#8154=VERTEX_POINT('',#31586);
#8155=VERTEX_POINT('',#31590);
#8156=VERTEX_POINT('',#31592);
#8157=VERTEX_POINT('',#31596);
#8158=VERTEX_POINT('',#31598);
#8159=VERTEX_POINT('',#31602);
#8160=VERTEX_POINT('',#31604);
#8161=VERTEX_POINT('',#31608);
#8162=VERTEX_POINT('',#31610);
#8163=VERTEX_POINT('',#31614);
#8164=VERTEX_POINT('',#31616);
#8165=VERTEX_POINT('',#31620);
#8166=VERTEX_POINT('',#31622);
#8167=VERTEX_POINT('',#31626);
#8168=VERTEX_POINT('',#31628);
#8169=VERTEX_POINT('',#31632);
#8170=VERTEX_POINT('',#31634);
#8171=VERTEX_POINT('',#31638);
#8172=VERTEX_POINT('',#31640);
#8173=VERTEX_POINT('',#31644);
#8174=VERTEX_POINT('',#31646);
#8175=VERTEX_POINT('',#31650);
#8176=VERTEX_POINT('',#31652);
#8177=VERTEX_POINT('',#31656);
#8178=VERTEX_POINT('',#31658);
#8179=VERTEX_POINT('',#31662);
#8180=VERTEX_POINT('',#31664);
#8181=VERTEX_POINT('',#31668);
#8182=VERTEX_POINT('',#31670);
#8183=VERTEX_POINT('',#31674);
#8184=VERTEX_POINT('',#31676);
#8185=VERTEX_POINT('',#31680);
#8186=VERTEX_POINT('',#31682);
#8187=VERTEX_POINT('',#31686);
#8188=VERTEX_POINT('',#31688);
#8189=VERTEX_POINT('',#31692);
#8190=VERTEX_POINT('',#31694);
#8191=VERTEX_POINT('',#31698);
#8192=VERTEX_POINT('',#31700);
#8193=VERTEX_POINT('',#31704);
#8194=VERTEX_POINT('',#31706);
#8195=VERTEX_POINT('',#31710);
#8196=VERTEX_POINT('',#31712);
#8197=VERTEX_POINT('',#31716);
#8198=VERTEX_POINT('',#31718);
#8199=VERTEX_POINT('',#31722);
#8200=VERTEX_POINT('',#31724);
#8201=VERTEX_POINT('',#31728);
#8202=VERTEX_POINT('',#31730);
#8203=VERTEX_POINT('',#31734);
#8204=VERTEX_POINT('',#31736);
#8205=VERTEX_POINT('',#31740);
#8206=VERTEX_POINT('',#31742);
#8207=VERTEX_POINT('',#31746);
#8208=VERTEX_POINT('',#31748);
#8209=VERTEX_POINT('',#31752);
#8210=VERTEX_POINT('',#31754);
#8211=VERTEX_POINT('',#31758);
#8212=VERTEX_POINT('',#31760);
#8213=VERTEX_POINT('',#31764);
#8214=VERTEX_POINT('',#31766);
#8215=VERTEX_POINT('',#31770);
#8216=VERTEX_POINT('',#31772);
#8217=VERTEX_POINT('',#31776);
#8218=VERTEX_POINT('',#31778);
#8219=VERTEX_POINT('',#31782);
#8220=VERTEX_POINT('',#31784);
#8221=VERTEX_POINT('',#31788);
#8222=VERTEX_POINT('',#31790);
#8223=VERTEX_POINT('',#31794);
#8224=VERTEX_POINT('',#31796);
#8225=VERTEX_POINT('',#31800);
#8226=VERTEX_POINT('',#31802);
#8227=VERTEX_POINT('',#31806);
#8228=VERTEX_POINT('',#31808);
#8229=VERTEX_POINT('',#31812);
#8230=VERTEX_POINT('',#31814);
#8231=VERTEX_POINT('',#31818);
#8232=VERTEX_POINT('',#31820);
#8233=VERTEX_POINT('',#31824);
#8234=VERTEX_POINT('',#31826);
#8235=VERTEX_POINT('',#31830);
#8236=VERTEX_POINT('',#31832);
#8237=VERTEX_POINT('',#31842);
#8238=VERTEX_POINT('',#31845);
#8239=VERTEX_POINT('',#31848);
#8240=VERTEX_POINT('',#31849);
#8241=VERTEX_POINT('',#32893);
#8242=VERTEX_POINT('',#32949);
#8243=VERTEX_POINT('',#32953);
#8244=VERTEX_POINT('',#32957);
#8245=VERTEX_POINT('',#32961);
#8246=VERTEX_POINT('',#32963);
#8247=VERTEX_POINT('',#32973);
#8248=VERTEX_POINT('',#32975);
#8249=VERTEX_POINT('',#32979);
#8250=VERTEX_POINT('',#32980);
#8251=VERTEX_POINT('',#32982);
#8252=VERTEX_POINT('',#32987);
#8253=VERTEX_POINT('',#32991);
#8254=VERTEX_POINT('',#32992);
#8255=VERTEX_POINT('',#32994);
#8256=VERTEX_POINT('',#32996);
#8257=VERTEX_POINT('',#32998);
#8258=VERTEX_POINT('',#33000);
#8259=VERTEX_POINT('',#33004);
#8260=VERTEX_POINT('',#33005);
#8261=VERTEX_POINT('',#33010);
#8262=VERTEX_POINT('',#33014);
#8263=VERTEX_POINT('',#33018);
#8264=VERTEX_POINT('',#33022);
#8265=VERTEX_POINT('',#33028);
#8266=VERTEX_POINT('',#33029);
#8267=VERTEX_POINT('',#33049);
#8268=VERTEX_POINT('',#33069);
#8269=VERTEX_POINT('',#33085);
#8270=VERTEX_POINT('',#33087);
#8271=VERTEX_POINT('',#33089);
#8272=VERTEX_POINT('',#33091);
#8273=VERTEX_POINT('',#33093);
#8274=VERTEX_POINT('',#33095);
#8275=VERTEX_POINT('',#33111);
#8276=VERTEX_POINT('',#33131);
#8277=VERTEX_POINT('',#33190);
#8278=VERTEX_POINT('',#33191);
#8279=VERTEX_POINT('',#33243);
#8280=VERTEX_POINT('',#33261);
#8281=VERTEX_POINT('',#33265);
#8282=VERTEX_POINT('',#33269);
#8283=VERTEX_POINT('',#33273);
#8284=VERTEX_POINT('',#33277);
#8285=VERTEX_POINT('',#33310);
#8286=VERTEX_POINT('',#33365);
#8287=VERTEX_POINT('',#33424);
#8288=VERTEX_POINT('',#33446);
#8289=VERTEX_POINT('',#33507);
#8290=VERTEX_POINT('',#33508);
#8291=VERTEX_POINT('',#33510);
#8292=VERTEX_POINT('',#33512);
#8293=VERTEX_POINT('',#33514);
#8294=VERTEX_POINT('',#33518);
#8295=VERTEX_POINT('',#33519);
#8296=VERTEX_POINT('',#33524);
#8297=VERTEX_POINT('',#33525);
#8298=VERTEX_POINT('',#33530);
#8299=VERTEX_POINT('',#33531);
#8300=VERTEX_POINT('',#33533);
#8301=VERTEX_POINT('',#33535);
#8302=VERTEX_POINT('',#33539);
#8303=VERTEX_POINT('',#33540);
#8304=VERTEX_POINT('',#33545);
#8305=VERTEX_POINT('',#33546);
#8306=VERTEX_POINT('',#33548);
#8307=VERTEX_POINT('',#33553);
#8308=VERTEX_POINT('',#33554);
#8309=VERTEX_POINT('',#33556);
#8310=VERTEX_POINT('',#33558);
#8311=VERTEX_POINT('',#33562);
#8312=VERTEX_POINT('',#33563);
#8313=VERTEX_POINT('',#33565);
#8314=VERTEX_POINT('',#33567);
#8315=VERTEX_POINT('',#33572);
#8316=VERTEX_POINT('',#33575);
#8317=VERTEX_POINT('',#33578);
#8318=VERTEX_POINT('',#33582);
#8319=VERTEX_POINT('',#33586);
#8320=VERTEX_POINT('',#33587);
#8321=VERTEX_POINT('',#33589);
#8322=VERTEX_POINT('',#33591);
#8323=VERTEX_POINT('',#33593);
#8324=VERTEX_POINT('',#33595);
#8325=VERTEX_POINT('',#33599);
#8326=VERTEX_POINT('',#33601);
#8327=VERTEX_POINT('',#33605);
#8328=VERTEX_POINT('',#33606);
#8329=VERTEX_POINT('',#33608);
#8330=VERTEX_POINT('',#33611);
#8331=VERTEX_POINT('',#33622);
#8332=VERTEX_POINT('',#33623);
#8333=VERTEX_POINT('',#33625);
#8334=VERTEX_POINT('',#33627);
#8335=VERTEX_POINT('',#33630);
#8336=VERTEX_POINT('',#33632);
#8337=VERTEX_POINT('',#33635);
#8338=VERTEX_POINT('',#33636);
#8339=VERTEX_POINT('',#33638);
#8340=VERTEX_POINT('',#33640);
#8341=VERTEX_POINT('',#33643);
#8342=VERTEX_POINT('',#33645);
#8343=VERTEX_POINT('',#33658);
#8344=VERTEX_POINT('',#33659);
#8345=VERTEX_POINT('',#33661);
#8346=VERTEX_POINT('',#33664);
#8347=VERTEX_POINT('',#33670);
#8348=VERTEX_POINT('',#33673);
#8349=VERTEX_POINT('',#33676);
#8350=VERTEX_POINT('',#33680);
#8351=VERTEX_POINT('',#33684);
#8352=VERTEX_POINT('',#33686);
#8353=VERTEX_POINT('',#33688);
#8354=VERTEX_POINT('',#33690);
#8355=VERTEX_POINT('',#33694);
#8356=VERTEX_POINT('',#33698);
#8357=VERTEX_POINT('',#33699);
#8358=VERTEX_POINT('',#33702);
#8359=VERTEX_POINT('',#33710);
#8360=VERTEX_POINT('',#33712);
#8361=VERTEX_POINT('',#33716);
#8362=VERTEX_POINT('',#33717);
#8363=VERTEX_POINT('',#33719);
#8364=VERTEX_POINT('',#33721);
#8365=VERTEX_POINT('',#33723);
#8366=VERTEX_POINT('',#33725);
#8367=VERTEX_POINT('',#33754);
#8368=VERTEX_POINT('',#33756);
#8369=VERTEX_POINT('',#33759);
#8370=VERTEX_POINT('',#33760);
#8371=VERTEX_POINT('',#33767);
#8372=VERTEX_POINT('',#33768);
#8373=VERTEX_POINT('',#33770);
#8374=VERTEX_POINT('',#33772);
#8375=VERTEX_POINT('',#33797);
#8376=VERTEX_POINT('',#33798);
#8377=VERTEX_POINT('',#33873);
#8378=VERTEX_POINT('',#33874);
#8379=VERTEX_POINT('',#33951);
#8380=VERTEX_POINT('',#33952);
#8381=VERTEX_POINT('',#34027);
#8382=VERTEX_POINT('',#34028);
#8383=VERTEX_POINT('',#34103);
#8384=VERTEX_POINT('',#34104);
#8385=VERTEX_POINT('',#34179);
#8386=VERTEX_POINT('',#34180);
#8387=VERTEX_POINT('',#34257);
#8388=VERTEX_POINT('',#34258);
#8389=VERTEX_POINT('',#34333);
#8390=VERTEX_POINT('',#34334);
#8391=VERTEX_POINT('',#34409);
#8392=VERTEX_POINT('',#34410);
#8393=VERTEX_POINT('',#34487);
#8394=VERTEX_POINT('',#34488);
#8395=VERTEX_POINT('',#34563);
#8396=VERTEX_POINT('',#34564);
#8397=VERTEX_POINT('',#34639);
#8398=VERTEX_POINT('',#34640);
#8399=VERTEX_POINT('',#34715);
#8400=VERTEX_POINT('',#34716);
#8401=VERTEX_POINT('',#34718);
#8402=VERTEX_POINT('',#34729);
#8403=VERTEX_POINT('',#34730);
#8404=VERTEX_POINT('',#34732);
#8405=VERTEX_POINT('',#34740);
#8406=VERTEX_POINT('',#34750);
#8407=VERTEX_POINT('',#34751);
#8408=VERTEX_POINT('',#34780);
#8409=VERTEX_POINT('',#34781);
#8410=VERTEX_POINT('',#34810);
#8411=VERTEX_POINT('',#34811);
#8412=VERTEX_POINT('',#34840);
#8413=VERTEX_POINT('',#34841);
#8414=VERTEX_POINT('',#34870);
#8415=VERTEX_POINT('',#34871);
#8416=VERTEX_POINT('',#34900);
#8417=VERTEX_POINT('',#34901);
#8418=VERTEX_POINT('',#34930);
#8419=VERTEX_POINT('',#34931);
#8420=VERTEX_POINT('',#34960);
#8421=VERTEX_POINT('',#34961);
#8422=VERTEX_POINT('',#34990);
#8423=VERTEX_POINT('',#34991);
#8424=VERTEX_POINT('',#35020);
#8425=VERTEX_POINT('',#35021);
#8426=VERTEX_POINT('',#35050);
#8427=VERTEX_POINT('',#35051);
#8428=VERTEX_POINT('',#35080);
#8429=VERTEX_POINT('',#35081);
#8430=VERTEX_POINT('',#35110);
#8431=VERTEX_POINT('',#35111);
#8432=VERTEX_POINT('',#35113);
#8433=VERTEX_POINT('',#35121);
#8434=VERTEX_POINT('',#35131);
#8435=VERTEX_POINT('',#35133);
#8436=VERTEX_POINT('',#35137);
#8437=VERTEX_POINT('',#35139);
#8438=VERTEX_POINT('',#35143);
#8439=VERTEX_POINT('',#35145);
#8440=VERTEX_POINT('',#35149);
#8441=VERTEX_POINT('',#35151);
#8442=VERTEX_POINT('',#35153);
#8443=VERTEX_POINT('',#35157);
#8444=VERTEX_POINT('',#35158);
#8445=VERTEX_POINT('',#35161);
#8446=VERTEX_POINT('',#35165);
#8447=VERTEX_POINT('',#35166);
#8448=VERTEX_POINT('',#35169);
#8449=VERTEX_POINT('',#35173);
#8450=VERTEX_POINT('',#35175);
#8451=VERTEX_POINT('',#35177);
#8452=VERTEX_POINT('',#35186);
#8453=VERTEX_POINT('',#35189);
#8454=VERTEX_POINT('',#35192);
#8455=VERTEX_POINT('',#35206);
#8456=VERTEX_POINT('',#35988);
#8457=VERTEX_POINT('',#36003);
#8458=VERTEX_POINT('',#36009);
#8459=VERTEX_POINT('',#36010);
#8460=VERTEX_POINT('',#36013);
#8461=VERTEX_POINT('',#36020);
#8462=VERTEX_POINT('',#36022);
#8463=VERTEX_POINT('',#36026);
#8464=VERTEX_POINT('',#36028);
#8465=VERTEX_POINT('',#36034);
#8466=VERTEX_POINT('',#36038);
#8467=VERTEX_POINT('',#36039);
#8468=VERTEX_POINT('',#36041);
#8469=VERTEX_POINT('',#36043);
#8470=VERTEX_POINT('',#36047);
#8471=VERTEX_POINT('',#36049);
#8472=VERTEX_POINT('',#36053);
#8473=VERTEX_POINT('',#36054);
#8474=VERTEX_POINT('',#36056);
#8475=VERTEX_POINT('',#36058);
#8476=VERTEX_POINT('',#36060);
#8477=VERTEX_POINT('',#36062);
#8478=VERTEX_POINT('',#36064);
#8479=VERTEX_POINT('',#36066);
#8480=VERTEX_POINT('',#36068);
#8481=VERTEX_POINT('',#36070);
#8482=VERTEX_POINT('',#36072);
#8483=VERTEX_POINT('',#36074);
#8484=VERTEX_POINT('',#36076);
#8485=VERTEX_POINT('',#36078);
#8486=VERTEX_POINT('',#36082);
#8487=VERTEX_POINT('',#36083);
#8488=VERTEX_POINT('',#36085);
#8489=VERTEX_POINT('',#36087);
#8490=VERTEX_POINT('',#36091);
#8491=VERTEX_POINT('',#36092);
#8492=VERTEX_POINT('',#36094);
#8493=VERTEX_POINT('',#36096);
#8494=VERTEX_POINT('',#36098);
#8495=VERTEX_POINT('',#36100);
#8496=VERTEX_POINT('',#36102);
#8497=VERTEX_POINT('',#36104);
#8498=VERTEX_POINT('',#36106);
#8499=VERTEX_POINT('',#36108);
#8500=VERTEX_POINT('',#36110);
#8501=VERTEX_POINT('',#36112);
#8502=VERTEX_POINT('',#36114);
#8503=VERTEX_POINT('',#36116);
#8504=VERTEX_POINT('',#36119);
#8505=VERTEX_POINT('',#36121);
#8506=VERTEX_POINT('',#36122);
#8507=VERTEX_POINT('',#36124);
#8508=VERTEX_POINT('',#36126);
#8509=VERTEX_POINT('',#36128);
#8510=VERTEX_POINT('',#36130);
#8511=VERTEX_POINT('',#36134);
#8512=VERTEX_POINT('',#36136);
#8513=VERTEX_POINT('',#36138);
#8514=VERTEX_POINT('',#36142);
#8515=VERTEX_POINT('',#36144);
#8516=VERTEX_POINT('',#36146);
#8517=VERTEX_POINT('',#36166);
#8518=VERTEX_POINT('',#36168);
#8519=VERTEX_POINT('',#36170);
#8520=VERTEX_POINT('',#36173);
#8521=VERTEX_POINT('',#36175);
#8522=VERTEX_POINT('',#36177);
#8523=VERTEX_POINT('',#36181);
#8524=VERTEX_POINT('',#36182);
#8525=VERTEX_POINT('',#36186);
#8526=VERTEX_POINT('',#36188);
#8527=VERTEX_POINT('',#36190);
#8528=VERTEX_POINT('',#36193);
#8529=VERTEX_POINT('',#36197);
#8530=VERTEX_POINT('',#36198);
#8531=VERTEX_POINT('',#36200);
#8532=VERTEX_POINT('',#36203);
#8533=VERTEX_POINT('',#36205);
#8534=VERTEX_POINT('',#36207);
#8535=VERTEX_POINT('',#36242);
#8536=VERTEX_POINT('',#36244);
#8537=VERTEX_POINT('',#36248);
#8538=VERTEX_POINT('',#36252);
#8539=VERTEX_POINT('',#36256);
#8540=VERTEX_POINT('',#36260);
#8541=VERTEX_POINT('',#36266);
#8542=VERTEX_POINT('',#36267);
#8543=VERTEX_POINT('',#36269);
#8544=VERTEX_POINT('',#36271);
#8545=VERTEX_POINT('',#36273);
#8546=VERTEX_POINT('',#36275);
#8547=VERTEX_POINT('',#36293);
#8548=VERTEX_POINT('',#36296);
#8549=VERTEX_POINT('',#36300);
#8550=VERTEX_POINT('',#36301);
#8551=VERTEX_POINT('',#36303);
#8552=VERTEX_POINT('',#36305);
#8553=VERTEX_POINT('',#36309);
#8554=VERTEX_POINT('',#36311);
#8555=VERTEX_POINT('',#36315);
#8556=VERTEX_POINT('',#36317);
#8557=VERTEX_POINT('',#36321);
#8558=VERTEX_POINT('',#36323);
#8559=VERTEX_POINT('',#36327);
#8560=VERTEX_POINT('',#36329);
#8561=VERTEX_POINT('',#36333);
#8562=VERTEX_POINT('',#36335);
#8563=VERTEX_POINT('',#36339);
#8564=VERTEX_POINT('',#36341);
#8565=VERTEX_POINT('',#36345);
#8566=VERTEX_POINT('',#36347);
#8567=VERTEX_POINT('',#36351);
#8568=VERTEX_POINT('',#36353);
#8569=VERTEX_POINT('',#36357);
#8570=VERTEX_POINT('',#36359);
#8571=VERTEX_POINT('',#36363);
#8572=VERTEX_POINT('',#36365);
#8573=VERTEX_POINT('',#36369);
#8574=VERTEX_POINT('',#36371);
#8575=VERTEX_POINT('',#36375);
#8576=VERTEX_POINT('',#36377);
#8577=VERTEX_POINT('',#36381);
#8578=VERTEX_POINT('',#36383);
#8579=VERTEX_POINT('',#36387);
#8580=VERTEX_POINT('',#36389);
#8581=VERTEX_POINT('',#36393);
#8582=VERTEX_POINT('',#36395);
#8583=VERTEX_POINT('',#36399);
#8584=VERTEX_POINT('',#36401);
#8585=VERTEX_POINT('',#36405);
#8586=VERTEX_POINT('',#36407);
#8587=VERTEX_POINT('',#36411);
#8588=VERTEX_POINT('',#36413);
#8589=VERTEX_POINT('',#36417);
#8590=VERTEX_POINT('',#36419);
#8591=VERTEX_POINT('',#36423);
#8592=VERTEX_POINT('',#36425);
#8593=VERTEX_POINT('',#36429);
#8594=VERTEX_POINT('',#36431);
#8595=VERTEX_POINT('',#36435);
#8596=VERTEX_POINT('',#36437);
#8597=VERTEX_POINT('',#36441);
#8598=VERTEX_POINT('',#36443);
#8599=VERTEX_POINT('',#36447);
#8600=VERTEX_POINT('',#36449);
#8601=VERTEX_POINT('',#36453);
#8602=VERTEX_POINT('',#36455);
#8603=VERTEX_POINT('',#36459);
#8604=VERTEX_POINT('',#36461);
#8605=VERTEX_POINT('',#36465);
#8606=VERTEX_POINT('',#36467);
#8607=VERTEX_POINT('',#36471);
#8608=VERTEX_POINT('',#36473);
#8609=VERTEX_POINT('',#36477);
#8610=VERTEX_POINT('',#36479);
#8611=VERTEX_POINT('',#36483);
#8612=VERTEX_POINT('',#36485);
#8613=VERTEX_POINT('',#36489);
#8614=VERTEX_POINT('',#36491);
#8615=VERTEX_POINT('',#36495);
#8616=VERTEX_POINT('',#36497);
#8617=VERTEX_POINT('',#36501);
#8618=VERTEX_POINT('',#36503);
#8619=VERTEX_POINT('',#36507);
#8620=VERTEX_POINT('',#36509);
#8621=VERTEX_POINT('',#36513);
#8622=VERTEX_POINT('',#36515);
#8623=VERTEX_POINT('',#36519);
#8624=VERTEX_POINT('',#36521);
#8625=VERTEX_POINT('',#36525);
#8626=VERTEX_POINT('',#36527);
#8627=VERTEX_POINT('',#36531);
#8628=VERTEX_POINT('',#36533);
#8629=VERTEX_POINT('',#36537);
#8630=VERTEX_POINT('',#36539);
#8631=VERTEX_POINT('',#36543);
#8632=VERTEX_POINT('',#36545);
#8633=VERTEX_POINT('',#36549);
#8634=VERTEX_POINT('',#36551);
#8635=VERTEX_POINT('',#36562);
#8636=VERTEX_POINT('',#36564);
#8637=VERTEX_POINT('',#36568);
#8638=VERTEX_POINT('',#36569);
#8639=VERTEX_POINT('',#36571);
#8640=VERTEX_POINT('',#36573);
#8641=VERTEX_POINT('',#36577);
#8642=VERTEX_POINT('',#36579);
#8643=VERTEX_POINT('',#36583);
#8644=VERTEX_POINT('',#36585);
#8645=VERTEX_POINT('',#36589);
#8646=VERTEX_POINT('',#36591);
#8647=VERTEX_POINT('',#36595);
#8648=VERTEX_POINT('',#36597);
#8649=VERTEX_POINT('',#36601);
#8650=VERTEX_POINT('',#36603);
#8651=VERTEX_POINT('',#36607);
#8652=VERTEX_POINT('',#36609);
#8653=VERTEX_POINT('',#36613);
#8654=VERTEX_POINT('',#36615);
#8655=VERTEX_POINT('',#36619);
#8656=VERTEX_POINT('',#36621);
#8657=VERTEX_POINT('',#36625);
#8658=VERTEX_POINT('',#36627);
#8659=EDGE_CURVE('',#7006,#7007,#3586,.T.);
#8660=EDGE_CURVE('',#7006,#7008,#3587,.T.);
#8661=EDGE_CURVE('',#7009,#7008,#3588,.T.);
#8662=EDGE_CURVE('',#7007,#7009,#3589,.T.);
#8663=EDGE_CURVE('',#7010,#7010,#973,.T.);
#8664=EDGE_CURVE('',#7011,#7011,#974,.T.);
#8665=EDGE_CURVE('',#7012,#7012,#975,.T.);
#8666=EDGE_CURVE('',#7013,#7013,#976,.T.);
#8667=EDGE_CURVE('',#7014,#7014,#977,.T.);
#8668=EDGE_CURVE('',#7015,#7015,#978,.T.);
#8669=EDGE_CURVE('',#7016,#7016,#979,.T.);
#8670=EDGE_CURVE('',#7017,#7017,#980,.T.);
#8671=EDGE_CURVE('',#7018,#7018,#981,.T.);
#8672=EDGE_CURVE('',#7019,#7019,#982,.T.);
#8673=EDGE_CURVE('',#7020,#7020,#983,.T.);
#8674=EDGE_CURVE('',#7021,#7021,#984,.T.);
#8675=EDGE_CURVE('',#7022,#7022,#985,.T.);
#8676=EDGE_CURVE('',#7023,#7023,#986,.T.);
#8677=EDGE_CURVE('',#7024,#7024,#987,.T.);
#8678=EDGE_CURVE('',#7025,#7025,#988,.T.);
#8679=EDGE_CURVE('',#7026,#7026,#989,.T.);
#8680=EDGE_CURVE('',#7027,#7027,#990,.T.);
#8681=EDGE_CURVE('',#7028,#7028,#991,.T.);
#8682=EDGE_CURVE('',#7029,#7029,#992,.T.);
#8683=EDGE_CURVE('',#7030,#7030,#993,.T.);
#8684=EDGE_CURVE('',#7031,#7031,#994,.T.);
#8685=EDGE_CURVE('',#7032,#7032,#995,.T.);
#8686=EDGE_CURVE('',#7033,#7033,#996,.T.);
#8687=EDGE_CURVE('',#7034,#7034,#997,.T.);
#8688=EDGE_CURVE('',#7035,#7035,#998,.T.);
#8689=EDGE_CURVE('',#7036,#7037,#3590,.T.);
#8690=EDGE_CURVE('',#7037,#7038,#3591,.T.);
#8691=EDGE_CURVE('',#7039,#7038,#3592,.T.);
#8692=EDGE_CURVE('',#7036,#7039,#3593,.T.);
#8693=EDGE_CURVE('',#7040,#7041,#3594,.T.);
#8694=EDGE_CURVE('',#7041,#7042,#3595,.T.);
#8695=EDGE_CURVE('',#7043,#7042,#3596,.T.);
#8696=EDGE_CURVE('',#7040,#7043,#3597,.T.);
#8697=EDGE_CURVE('',#7044,#7045,#3598,.T.);
#8698=EDGE_CURVE('',#7045,#7046,#3599,.T.);
#8699=EDGE_CURVE('',#7047,#7046,#3600,.T.);
#8700=EDGE_CURVE('',#7044,#7047,#3601,.T.);
#8701=EDGE_CURVE('',#7048,#7049,#3602,.T.);
#8702=EDGE_CURVE('',#7049,#7050,#3603,.T.);
#8703=EDGE_CURVE('',#7051,#7050,#3604,.T.);
#8704=EDGE_CURVE('',#7048,#7051,#3605,.T.);
#8705=EDGE_CURVE('',#7052,#7053,#3606,.T.);
#8706=EDGE_CURVE('',#7053,#7054,#3607,.T.);
#8707=EDGE_CURVE('',#7055,#7054,#3608,.T.);
#8708=EDGE_CURVE('',#7052,#7055,#3609,.T.);
#8709=EDGE_CURVE('',#7056,#7057,#3610,.T.);
#8710=EDGE_CURVE('',#7057,#7058,#3611,.T.);
#8711=EDGE_CURVE('',#7059,#7058,#3612,.T.);
#8712=EDGE_CURVE('',#7056,#7059,#3613,.T.);
#8713=EDGE_CURVE('',#7060,#7061,#3614,.T.);
#8714=EDGE_CURVE('',#7061,#7062,#3615,.T.);
#8715=EDGE_CURVE('',#7063,#7062,#3616,.T.);
#8716=EDGE_CURVE('',#7060,#7063,#3617,.T.);
#8717=EDGE_CURVE('',#7064,#7065,#3618,.T.);
#8718=EDGE_CURVE('',#7065,#7066,#3619,.T.);
#8719=EDGE_CURVE('',#7067,#7066,#3620,.T.);
#8720=EDGE_CURVE('',#7064,#7067,#3621,.T.);
#8721=EDGE_CURVE('',#7068,#7069,#3622,.T.);
#8722=EDGE_CURVE('',#7069,#7070,#3623,.T.);
#8723=EDGE_CURVE('',#7071,#7070,#3624,.T.);
#8724=EDGE_CURVE('',#7068,#7071,#3625,.T.);
#8725=EDGE_CURVE('',#7072,#7073,#3626,.T.);
#8726=EDGE_CURVE('',#7073,#7074,#3627,.T.);
#8727=EDGE_CURVE('',#7075,#7074,#3628,.T.);
#8728=EDGE_CURVE('',#7072,#7075,#3629,.T.);
#8729=EDGE_CURVE('',#7076,#7077,#3630,.T.);
#8730=EDGE_CURVE('',#7077,#7078,#3631,.T.);
#8731=EDGE_CURVE('',#7079,#7078,#3632,.T.);
#8732=EDGE_CURVE('',#7076,#7079,#3633,.T.);
#8733=EDGE_CURVE('',#7080,#7081,#3634,.T.);
#8734=EDGE_CURVE('',#7081,#7082,#3635,.T.);
#8735=EDGE_CURVE('',#7083,#7082,#3636,.T.);
#8736=EDGE_CURVE('',#7080,#7083,#3637,.T.);
#8737=EDGE_CURVE('',#7084,#7085,#3638,.T.);
#8738=EDGE_CURVE('',#7085,#7086,#3639,.T.);
#8739=EDGE_CURVE('',#7087,#7086,#3640,.T.);
#8740=EDGE_CURVE('',#7084,#7087,#3641,.T.);
#8741=EDGE_CURVE('',#7088,#7089,#3642,.T.);
#8742=EDGE_CURVE('',#7089,#7090,#3643,.T.);
#8743=EDGE_CURVE('',#7091,#7090,#3644,.T.);
#8744=EDGE_CURVE('',#7088,#7091,#3645,.T.);
#8745=EDGE_CURVE('',#7092,#7093,#3646,.T.);
#8746=EDGE_CURVE('',#7093,#7094,#3647,.T.);
#8747=EDGE_CURVE('',#7095,#7094,#3648,.T.);
#8748=EDGE_CURVE('',#7092,#7095,#3649,.T.);
#8749=EDGE_CURVE('',#7096,#7097,#3650,.T.);
#8750=EDGE_CURVE('',#7097,#7098,#3651,.T.);
#8751=EDGE_CURVE('',#7099,#7098,#3652,.T.);
#8752=EDGE_CURVE('',#7096,#7099,#3653,.T.);
#8753=EDGE_CURVE('',#7100,#7101,#3654,.T.);
#8754=EDGE_CURVE('',#7101,#7102,#3655,.T.);
#8755=EDGE_CURVE('',#7103,#7102,#3656,.T.);
#8756=EDGE_CURVE('',#7100,#7103,#3657,.T.);
#8757=EDGE_CURVE('',#7104,#7105,#3658,.T.);
#8758=EDGE_CURVE('',#7105,#7106,#3659,.T.);
#8759=EDGE_CURVE('',#7107,#7106,#3660,.T.);
#8760=EDGE_CURVE('',#7104,#7107,#3661,.T.);
#8761=EDGE_CURVE('',#7108,#7109,#3662,.T.);
#8762=EDGE_CURVE('',#7109,#7110,#3663,.T.);
#8763=EDGE_CURVE('',#7111,#7110,#3664,.T.);
#8764=EDGE_CURVE('',#7108,#7111,#3665,.T.);
#8765=EDGE_CURVE('',#7112,#7113,#3666,.T.);
#8766=EDGE_CURVE('',#7113,#7114,#3667,.T.);
#8767=EDGE_CURVE('',#7115,#7114,#3668,.T.);
#8768=EDGE_CURVE('',#7112,#7115,#3669,.T.);
#8769=EDGE_CURVE('',#7116,#7117,#3670,.T.);
#8770=EDGE_CURVE('',#7117,#7118,#3671,.T.);
#8771=EDGE_CURVE('',#7119,#7118,#3672,.T.);
#8772=EDGE_CURVE('',#7116,#7119,#3673,.T.);
#8773=EDGE_CURVE('',#7120,#7121,#3674,.T.);
#8774=EDGE_CURVE('',#7121,#7122,#3675,.T.);
#8775=EDGE_CURVE('',#7123,#7122,#3676,.T.);
#8776=EDGE_CURVE('',#7120,#7123,#3677,.T.);
#8777=EDGE_CURVE('',#7124,#7125,#3678,.T.);
#8778=EDGE_CURVE('',#7125,#7126,#3679,.T.);
#8779=EDGE_CURVE('',#7127,#7126,#3680,.T.);
#8780=EDGE_CURVE('',#7124,#7127,#3681,.T.);
#8781=EDGE_CURVE('',#7128,#7129,#3682,.T.);
#8782=EDGE_CURVE('',#7129,#7130,#3683,.T.);
#8783=EDGE_CURVE('',#7131,#7130,#3684,.T.);
#8784=EDGE_CURVE('',#7128,#7131,#3685,.T.);
#8785=EDGE_CURVE('',#7132,#7133,#3686,.T.);
#8786=EDGE_CURVE('',#7133,#7134,#3687,.T.);
#8787=EDGE_CURVE('',#7135,#7134,#3688,.T.);
#8788=EDGE_CURVE('',#7132,#7135,#3689,.T.);
#8789=EDGE_CURVE('',#7136,#7137,#3690,.T.);
#8790=EDGE_CURVE('',#7137,#7138,#3691,.T.);
#8791=EDGE_CURVE('',#7139,#7138,#3692,.T.);
#8792=EDGE_CURVE('',#7136,#7139,#3693,.T.);
#8793=EDGE_CURVE('',#7140,#7141,#3694,.T.);
#8794=EDGE_CURVE('',#7140,#7142,#3695,.T.);
#8795=EDGE_CURVE('',#7142,#7143,#3696,.T.);
#8796=EDGE_CURVE('',#7141,#7143,#3697,.T.);
#8797=EDGE_CURVE('',#7144,#7145,#3698,.T.);
#8798=EDGE_CURVE('',#7144,#7146,#3699,.T.);
#8799=EDGE_CURVE('',#7146,#7147,#3700,.T.);
#8800=EDGE_CURVE('',#7145,#7147,#3701,.T.);
#8801=EDGE_CURVE('',#7148,#7149,#3702,.T.);
#8802=EDGE_CURVE('',#7148,#7150,#3703,.T.);
#8803=EDGE_CURVE('',#7150,#7151,#3704,.T.);
#8804=EDGE_CURVE('',#7149,#7151,#3705,.T.);
#8805=EDGE_CURVE('',#7152,#7153,#3706,.T.);
#8806=EDGE_CURVE('',#7152,#7154,#3707,.T.);
#8807=EDGE_CURVE('',#7154,#7155,#3708,.T.);
#8808=EDGE_CURVE('',#7153,#7155,#3709,.T.);
#8809=EDGE_CURVE('',#7156,#7157,#3710,.T.);
#8810=EDGE_CURVE('',#7156,#7158,#3711,.T.);
#8811=EDGE_CURVE('',#7158,#7159,#3712,.T.);
#8812=EDGE_CURVE('',#7157,#7159,#3713,.T.);
#8813=EDGE_CURVE('',#7160,#7161,#3714,.T.);
#8814=EDGE_CURVE('',#7160,#7162,#3715,.T.);
#8815=EDGE_CURVE('',#7162,#7163,#3716,.T.);
#8816=EDGE_CURVE('',#7161,#7163,#3717,.T.);
#8817=EDGE_CURVE('',#7164,#7165,#3718,.T.);
#8818=EDGE_CURVE('',#7164,#7166,#3719,.T.);
#8819=EDGE_CURVE('',#7166,#7167,#3720,.T.);
#8820=EDGE_CURVE('',#7165,#7167,#3721,.T.);
#8821=EDGE_CURVE('',#7168,#7169,#3722,.T.);
#8822=EDGE_CURVE('',#7168,#7170,#3723,.T.);
#8823=EDGE_CURVE('',#7170,#7171,#3724,.T.);
#8824=EDGE_CURVE('',#7169,#7171,#3725,.T.);
#8825=EDGE_CURVE('',#7172,#7173,#3726,.T.);
#8826=EDGE_CURVE('',#7172,#7174,#3727,.T.);
#8827=EDGE_CURVE('',#7174,#7175,#3728,.T.);
#8828=EDGE_CURVE('',#7173,#7175,#3729,.T.);
#8829=EDGE_CURVE('',#7176,#7177,#3730,.T.);
#8830=EDGE_CURVE('',#7176,#7178,#3731,.T.);
#8831=EDGE_CURVE('',#7178,#7179,#3732,.T.);
#8832=EDGE_CURVE('',#7177,#7179,#3733,.T.);
#8833=EDGE_CURVE('',#7180,#7181,#3734,.T.);
#8834=EDGE_CURVE('',#7180,#7182,#3735,.T.);
#8835=EDGE_CURVE('',#7182,#7183,#3736,.T.);
#8836=EDGE_CURVE('',#7181,#7183,#3737,.T.);
#8837=EDGE_CURVE('',#7184,#7185,#3738,.T.);
#8838=EDGE_CURVE('',#7184,#7186,#3739,.T.);
#8839=EDGE_CURVE('',#7186,#7187,#3740,.T.);
#8840=EDGE_CURVE('',#7185,#7187,#3741,.T.);
#8841=EDGE_CURVE('',#7188,#7189,#3742,.T.);
#8842=EDGE_CURVE('',#7188,#7190,#3743,.T.);
#8843=EDGE_CURVE('',#7190,#7191,#3744,.T.);
#8844=EDGE_CURVE('',#7189,#7191,#3745,.T.);
#8845=EDGE_CURVE('',#7192,#7193,#3746,.T.);
#8846=EDGE_CURVE('',#7192,#7194,#3747,.T.);
#8847=EDGE_CURVE('',#7194,#7195,#3748,.T.);
#8848=EDGE_CURVE('',#7193,#7195,#3749,.T.);
#8849=EDGE_CURVE('',#7196,#7197,#3750,.T.);
#8850=EDGE_CURVE('',#7196,#7198,#3751,.T.);
#8851=EDGE_CURVE('',#7198,#7199,#3752,.T.);
#8852=EDGE_CURVE('',#7197,#7199,#3753,.T.);
#8853=EDGE_CURVE('',#7200,#7201,#3754,.T.);
#8854=EDGE_CURVE('',#7200,#7202,#3755,.T.);
#8855=EDGE_CURVE('',#7202,#7203,#3756,.T.);
#8856=EDGE_CURVE('',#7201,#7203,#3757,.T.);
#8857=EDGE_CURVE('',#7204,#7205,#3758,.T.);
#8858=EDGE_CURVE('',#7204,#7206,#3759,.T.);
#8859=EDGE_CURVE('',#7206,#7207,#3760,.T.);
#8860=EDGE_CURVE('',#7205,#7207,#3761,.T.);
#8861=EDGE_CURVE('',#7208,#7209,#3762,.T.);
#8862=EDGE_CURVE('',#7208,#7210,#3763,.T.);
#8863=EDGE_CURVE('',#7210,#7211,#3764,.T.);
#8864=EDGE_CURVE('',#7209,#7211,#3765,.T.);
#8865=EDGE_CURVE('',#7212,#7213,#3766,.T.);
#8866=EDGE_CURVE('',#7212,#7214,#3767,.T.);
#8867=EDGE_CURVE('',#7214,#7215,#3768,.T.);
#8868=EDGE_CURVE('',#7213,#7215,#3769,.T.);
#8869=EDGE_CURVE('',#7216,#7217,#3770,.T.);
#8870=EDGE_CURVE('',#7216,#7218,#3771,.T.);
#8871=EDGE_CURVE('',#7218,#7219,#3772,.T.);
#8872=EDGE_CURVE('',#7217,#7219,#3773,.T.);
#8873=EDGE_CURVE('',#7220,#7221,#3774,.T.);
#8874=EDGE_CURVE('',#7220,#7222,#3775,.T.);
#8875=EDGE_CURVE('',#7222,#7223,#3776,.T.);
#8876=EDGE_CURVE('',#7221,#7223,#3777,.T.);
#8877=EDGE_CURVE('',#7224,#7225,#3778,.T.);
#8878=EDGE_CURVE('',#7224,#7226,#3779,.T.);
#8879=EDGE_CURVE('',#7226,#7227,#3780,.T.);
#8880=EDGE_CURVE('',#7225,#7227,#3781,.T.);
#8881=EDGE_CURVE('',#7228,#7229,#3782,.T.);
#8882=EDGE_CURVE('',#7228,#7230,#3783,.T.);
#8883=EDGE_CURVE('',#7230,#7231,#3784,.T.);
#8884=EDGE_CURVE('',#7229,#7231,#3785,.T.);
#8885=EDGE_CURVE('',#7232,#7233,#3786,.T.);
#8886=EDGE_CURVE('',#7232,#7234,#3787,.T.);
#8887=EDGE_CURVE('',#7234,#7235,#3788,.T.);
#8888=EDGE_CURVE('',#7233,#7235,#3789,.T.);
#8889=EDGE_CURVE('',#7236,#7237,#3790,.T.);
#8890=EDGE_CURVE('',#7236,#7238,#3791,.T.);
#8891=EDGE_CURVE('',#7238,#7239,#3792,.T.);
#8892=EDGE_CURVE('',#7237,#7239,#3793,.T.);
#8893=EDGE_CURVE('',#7240,#7241,#3794,.T.);
#8894=EDGE_CURVE('',#7240,#7242,#3795,.T.);
#8895=EDGE_CURVE('',#7242,#7243,#3796,.T.);
#8896=EDGE_CURVE('',#7241,#7243,#3797,.T.);
#8897=EDGE_CURVE('',#7244,#7245,#3798,.T.);
#8898=EDGE_CURVE('',#7244,#7246,#3799,.T.);
#8899=EDGE_CURVE('',#7246,#7247,#3800,.T.);
#8900=EDGE_CURVE('',#7245,#7247,#3801,.T.);
#8901=EDGE_CURVE('',#7248,#7248,#999,.T.);
#8902=EDGE_CURVE('',#7249,#7249,#1000,.T.);
#8903=EDGE_CURVE('',#7250,#7250,#1001,.T.);
#8904=EDGE_CURVE('',#7251,#7251,#1002,.T.);
#8905=EDGE_CURVE('',#7252,#7252,#1003,.T.);
#8906=EDGE_CURVE('',#7253,#7253,#1004,.T.);
#8907=EDGE_CURVE('',#7254,#7254,#1005,.T.);
#8908=EDGE_CURVE('',#7255,#7255,#1006,.T.);
#8909=EDGE_CURVE('',#7256,#7256,#1007,.T.);
#8910=EDGE_CURVE('',#7257,#7257,#1008,.T.);
#8911=EDGE_CURVE('',#7258,#7258,#1009,.T.);
#8912=EDGE_CURVE('',#7259,#7259,#1010,.T.);
#8913=EDGE_CURVE('',#7260,#7260,#1011,.T.);
#8914=EDGE_CURVE('',#7261,#7261,#1012,.T.);
#8915=EDGE_CURVE('',#7262,#7262,#1013,.T.);
#8916=EDGE_CURVE('',#7263,#7263,#1014,.T.);
#8917=EDGE_CURVE('',#7264,#7264,#1015,.T.);
#8918=EDGE_CURVE('',#7265,#7265,#1016,.T.);
#8919=EDGE_CURVE('',#7266,#7266,#1017,.T.);
#8920=EDGE_CURVE('',#7267,#7267,#1018,.T.);
#8921=EDGE_CURVE('',#7268,#7268,#1019,.T.);
#8922=EDGE_CURVE('',#7269,#7269,#1020,.T.);
#8923=EDGE_CURVE('',#7270,#7270,#1021,.T.);
#8924=EDGE_CURVE('',#7271,#7271,#1022,.T.);
#8925=EDGE_CURVE('',#7272,#7272,#1023,.T.);
#8926=EDGE_CURVE('',#7273,#7273,#1024,.T.);
#8927=EDGE_CURVE('',#7145,#7137,#3802,.T.);
#8928=EDGE_CURVE('',#7147,#7138,#3803,.T.);
#8929=EDGE_CURVE('',#7273,#7010,#3804,.T.);
#8930=EDGE_CURVE('',#7272,#7011,#3805,.T.);
#8931=EDGE_CURVE('',#7271,#7012,#3806,.T.);
#8932=EDGE_CURVE('',#7270,#7013,#3807,.T.);
#8933=EDGE_CURVE('',#7269,#7014,#3808,.T.);
#8934=EDGE_CURVE('',#7268,#7015,#3809,.T.);
#8935=EDGE_CURVE('',#7267,#7016,#3810,.T.);
#8936=EDGE_CURVE('',#7266,#7017,#3811,.T.);
#8937=EDGE_CURVE('',#7265,#7018,#3812,.T.);
#8938=EDGE_CURVE('',#7264,#7019,#3813,.T.);
#8939=EDGE_CURVE('',#7263,#7020,#3814,.T.);
#8940=EDGE_CURVE('',#7262,#7021,#3815,.T.);
#8941=EDGE_CURVE('',#7261,#7022,#3816,.T.);
#8942=EDGE_CURVE('',#7260,#7023,#3817,.T.);
#8943=EDGE_CURVE('',#7259,#7024,#3818,.T.);
#8944=EDGE_CURVE('',#7258,#7025,#3819,.T.);
#8945=EDGE_CURVE('',#7257,#7026,#3820,.T.);
#8946=EDGE_CURVE('',#7256,#7027,#3821,.T.);
#8947=EDGE_CURVE('',#7255,#7028,#3822,.T.);
#8948=EDGE_CURVE('',#7254,#7029,#3823,.T.);
#8949=EDGE_CURVE('',#7253,#7030,#3824,.T.);
#8950=EDGE_CURVE('',#7252,#7031,#3825,.T.);
#8951=EDGE_CURVE('',#7251,#7032,#3826,.T.);
#8952=EDGE_CURVE('',#7250,#7033,#3827,.T.);
#8953=EDGE_CURVE('',#7249,#7034,#3828,.T.);
#8954=EDGE_CURVE('',#7248,#7035,#3829,.T.);
#8955=EDGE_CURVE('',#7245,#7037,#3830,.T.);
#8956=EDGE_CURVE('',#7247,#7038,#3831,.T.);
#8957=EDGE_CURVE('',#7241,#7041,#3832,.T.);
#8958=EDGE_CURVE('',#7243,#7042,#3833,.T.);
#8959=EDGE_CURVE('',#7237,#7045,#3834,.T.);
#8960=EDGE_CURVE('',#7239,#7046,#3835,.T.);
#8961=EDGE_CURVE('',#7233,#7049,#3836,.T.);
#8962=EDGE_CURVE('',#7235,#7050,#3837,.T.);
#8963=EDGE_CURVE('',#7229,#7053,#3838,.T.);
#8964=EDGE_CURVE('',#7231,#7054,#3839,.T.);
#8965=EDGE_CURVE('',#7225,#7057,#3840,.T.);
#8966=EDGE_CURVE('',#7227,#7058,#3841,.T.);
#8967=EDGE_CURVE('',#7221,#7061,#3842,.T.);
#8968=EDGE_CURVE('',#7223,#7062,#3843,.T.);
#8969=EDGE_CURVE('',#7217,#7065,#3844,.T.);
#8970=EDGE_CURVE('',#7219,#7066,#3845,.T.);
#8971=EDGE_CURVE('',#7213,#7069,#3846,.T.);
#8972=EDGE_CURVE('',#7215,#7070,#3847,.T.);
#8973=EDGE_CURVE('',#7209,#7073,#3848,.T.);
#8974=EDGE_CURVE('',#7211,#7074,#3849,.T.);
#8975=EDGE_CURVE('',#7205,#7077,#3850,.T.);
#8976=EDGE_CURVE('',#7207,#7078,#3851,.T.);
#8977=EDGE_CURVE('',#7201,#7081,#3852,.T.);
#8978=EDGE_CURVE('',#7203,#7082,#3853,.T.);
#8979=EDGE_CURVE('',#7197,#7085,#3854,.T.);
#8980=EDGE_CURVE('',#7199,#7086,#3855,.T.);
#8981=EDGE_CURVE('',#7193,#7089,#3856,.T.);
#8982=EDGE_CURVE('',#7195,#7090,#3857,.T.);
#8983=EDGE_CURVE('',#7189,#7093,#3858,.T.);
#8984=EDGE_CURVE('',#7191,#7094,#3859,.T.);
#8985=EDGE_CURVE('',#7185,#7097,#3860,.T.);
#8986=EDGE_CURVE('',#7187,#7098,#3861,.T.);
#8987=EDGE_CURVE('',#7181,#7101,#3862,.T.);
#8988=EDGE_CURVE('',#7183,#7102,#3863,.T.);
#8989=EDGE_CURVE('',#7177,#7105,#3864,.T.);
#8990=EDGE_CURVE('',#7179,#7106,#3865,.T.);
#8991=EDGE_CURVE('',#7173,#7109,#3866,.T.);
#8992=EDGE_CURVE('',#7175,#7110,#3867,.T.);
#8993=EDGE_CURVE('',#7169,#7113,#3868,.T.);
#8994=EDGE_CURVE('',#7171,#7114,#3869,.T.);
#8995=EDGE_CURVE('',#7165,#7117,#3870,.T.);
#8996=EDGE_CURVE('',#7167,#7118,#3871,.T.);
#8997=EDGE_CURVE('',#7161,#7121,#3872,.T.);
#8998=EDGE_CURVE('',#7163,#7122,#3873,.T.);
#8999=EDGE_CURVE('',#7157,#7125,#3874,.T.);
#9000=EDGE_CURVE('',#7159,#7126,#3875,.T.);
#9001=EDGE_CURVE('',#7153,#7129,#3876,.T.);
#9002=EDGE_CURVE('',#7155,#7130,#3877,.T.);
#9003=EDGE_CURVE('',#7149,#7133,#3878,.T.);
#9004=EDGE_CURVE('',#7151,#7134,#3879,.T.);
#9005=EDGE_CURVE('',#7141,#7006,#3880,.T.);
#9006=EDGE_CURVE('',#7143,#7008,#3881,.T.);
#9007=EDGE_CURVE('',#7142,#7009,#3882,.T.);
#9008=EDGE_CURVE('',#7140,#7007,#3883,.T.);
#9009=EDGE_CURVE('',#7246,#7039,#3884,.T.);
#9010=EDGE_CURVE('',#7244,#7036,#3885,.T.);
#9011=EDGE_CURVE('',#7242,#7043,#3886,.T.);
#9012=EDGE_CURVE('',#7240,#7040,#3887,.T.);
#9013=EDGE_CURVE('',#7238,#7047,#3888,.T.);
#9014=EDGE_CURVE('',#7236,#7044,#3889,.T.);
#9015=EDGE_CURVE('',#7234,#7051,#3890,.T.);
#9016=EDGE_CURVE('',#7232,#7048,#3891,.T.);
#9017=EDGE_CURVE('',#7230,#7055,#3892,.T.);
#9018=EDGE_CURVE('',#7228,#7052,#3893,.T.);
#9019=EDGE_CURVE('',#7226,#7059,#3894,.T.);
#9020=EDGE_CURVE('',#7224,#7056,#3895,.T.);
#9021=EDGE_CURVE('',#7222,#7063,#3896,.T.);
#9022=EDGE_CURVE('',#7220,#7060,#3897,.T.);
#9023=EDGE_CURVE('',#7218,#7067,#3898,.T.);
#9024=EDGE_CURVE('',#7216,#7064,#3899,.T.);
#9025=EDGE_CURVE('',#7214,#7071,#3900,.T.);
#9026=EDGE_CURVE('',#7212,#7068,#3901,.T.);
#9027=EDGE_CURVE('',#7210,#7075,#3902,.T.);
#9028=EDGE_CURVE('',#7208,#7072,#3903,.T.);
#9029=EDGE_CURVE('',#7206,#7079,#3904,.T.);
#9030=EDGE_CURVE('',#7204,#7076,#3905,.T.);
#9031=EDGE_CURVE('',#7202,#7083,#3906,.T.);
#9032=EDGE_CURVE('',#7200,#7080,#3907,.T.);
#9033=EDGE_CURVE('',#7198,#7087,#3908,.T.);
#9034=EDGE_CURVE('',#7196,#7084,#3909,.T.);
#9035=EDGE_CURVE('',#7194,#7091,#3910,.T.);
#9036=EDGE_CURVE('',#7192,#7088,#3911,.T.);
#9037=EDGE_CURVE('',#7190,#7095,#3912,.T.);
#9038=EDGE_CURVE('',#7188,#7092,#3913,.T.);
#9039=EDGE_CURVE('',#7186,#7099,#3914,.T.);
#9040=EDGE_CURVE('',#7184,#7096,#3915,.T.);
#9041=EDGE_CURVE('',#7182,#7103,#3916,.T.);
#9042=EDGE_CURVE('',#7180,#7100,#3917,.T.);
#9043=EDGE_CURVE('',#7178,#7107,#3918,.T.);
#9044=EDGE_CURVE('',#7176,#7104,#3919,.T.);
#9045=EDGE_CURVE('',#7174,#7111,#3920,.T.);
#9046=EDGE_CURVE('',#7172,#7108,#3921,.T.);
#9047=EDGE_CURVE('',#7170,#7115,#3922,.T.);
#9048=EDGE_CURVE('',#7168,#7112,#3923,.T.);
#9049=EDGE_CURVE('',#7166,#7119,#3924,.T.);
#9050=EDGE_CURVE('',#7164,#7116,#3925,.T.);
#9051=EDGE_CURVE('',#7162,#7123,#3926,.T.);
#9052=EDGE_CURVE('',#7160,#7120,#3927,.T.);
#9053=EDGE_CURVE('',#7158,#7127,#3928,.T.);
#9054=EDGE_CURVE('',#7156,#7124,#3929,.T.);
#9055=EDGE_CURVE('',#7154,#7131,#3930,.T.);
#9056=EDGE_CURVE('',#7152,#7128,#3931,.T.);
#9057=EDGE_CURVE('',#7150,#7135,#3932,.T.);
#9058=EDGE_CURVE('',#7148,#7132,#3933,.T.);
#9059=EDGE_CURVE('',#7146,#7139,#3934,.T.);
#9060=EDGE_CURVE('',#7144,#7136,#3935,.T.);
#9061=EDGE_CURVE('',#7274,#7275,#417,.T.);
#9062=EDGE_CURVE('',#7276,#7275,#418,.T.);
#9063=EDGE_CURVE('',#7277,#7276,#3936,.T.);
#9064=EDGE_CURVE('',#7278,#7277,#419,.T.);
#9065=EDGE_CURVE('',#7278,#7279,#420,.T.);
#9066=EDGE_CURVE('',#7274,#7279,#3937,.T.);
#9067=EDGE_CURVE('',#7279,#7277,#3938,.T.);
#9068=EDGE_CURVE('',#7276,#7274,#3939,.T.);
#9069=EDGE_CURVE('',#7280,#7281,#421,.T.);
#9070=EDGE_CURVE('',#7282,#7281,#422,.T.);
#9071=EDGE_CURVE('',#7283,#7282,#3940,.T.);
#9072=EDGE_CURVE('',#7284,#7283,#423,.T.);
#9073=EDGE_CURVE('',#7284,#7285,#424,.T.);
#9074=EDGE_CURVE('',#7280,#7285,#3941,.T.);
#9075=EDGE_CURVE('',#7285,#7283,#3942,.T.);
#9076=EDGE_CURVE('',#7282,#7280,#3943,.T.);
#9077=EDGE_CURVE('',#7286,#7287,#425,.T.);
#9078=EDGE_CURVE('',#7288,#7287,#426,.T.);
#9079=EDGE_CURVE('',#7289,#7288,#3944,.T.);
#9080=EDGE_CURVE('',#7290,#7289,#427,.T.);
#9081=EDGE_CURVE('',#7290,#7291,#428,.T.);
#9082=EDGE_CURVE('',#7286,#7291,#3945,.T.);
#9083=EDGE_CURVE('',#7291,#7289,#3946,.T.);
#9084=EDGE_CURVE('',#7288,#7286,#3947,.T.);
#9085=EDGE_CURVE('',#7292,#7293,#1025,.T.);
#9086=EDGE_CURVE('',#7294,#7292,#1026,.T.);
#9087=EDGE_CURVE('',#7294,#7295,#1027,.T.);
#9088=EDGE_CURVE('',#7293,#7295,#1028,.T.);
#9089=EDGE_CURVE('',#7296,#7297,#1029,.T.);
#9090=EDGE_CURVE('',#7298,#7297,#3948,.T.);
#9091=EDGE_CURVE('',#7295,#7298,#1030,.T.);
#9092=EDGE_CURVE('',#7296,#7294,#3949,.T.);
#9093=EDGE_CURVE('',#7296,#7297,#1031,.T.);
#9094=EDGE_CURVE('',#7299,#7300,#1032,.T.);
#9095=EDGE_CURVE('',#7301,#7300,#3950,.T.);
#9096=EDGE_CURVE('',#7301,#7302,#3951,.T.);
#9097=EDGE_CURVE('',#7297,#7302,#3952,.T.);
#9098=EDGE_CURVE('',#7303,#7296,#3953,.T.);
#9099=EDGE_CURVE('',#7304,#7303,#3954,.T.);
#9100=EDGE_CURVE('',#7299,#7304,#3955,.T.);
#9101=EDGE_CURVE('',#7299,#7300,#1033,.T.);
#9102=EDGE_CURVE('',#7305,#7306,#1034,.T.);
#9103=EDGE_CURVE('',#7307,#7306,#1035,.T.);
#9104=EDGE_CURVE('',#7300,#7307,#3956,.T.);
#9105=EDGE_CURVE('',#7305,#7299,#3957,.T.);
#9106=EDGE_CURVE('',#7308,#7309,#1036,.T.);
#9107=EDGE_CURVE('',#7310,#7309,#1037,.T.);
#9108=EDGE_CURVE('',#7306,#7310,#1038,.T.);
#9109=EDGE_CURVE('',#7308,#7305,#1039,.T.);
#9110=EDGE_CURVE('',#7309,#7311,#3958,.T.);
#9111=EDGE_CURVE('',#7312,#7308,#3959,.T.);
#9112=EDGE_CURVE('',#7311,#7312,#1040,.T.);
#9113=EDGE_CURVE('',#7313,#7314,#3960,.T.);
#9114=EDGE_CURVE('',#7315,#7314,#1041,.T.);
#9115=EDGE_CURVE('',#7315,#7316,#3961,.T.);
#9116=EDGE_CURVE('',#7316,#7317,#3962,.T.);
#9117=EDGE_CURVE('',#7313,#7317,#3963,.T.);
#9118=EDGE_CURVE('',#7318,#7313,#3964,.T.);
#9119=EDGE_CURVE('',#7317,#7319,#3965,.T.);
#9120=EDGE_CURVE('',#7318,#7319,#3966,.T.);
#9121=EDGE_CURVE('',#7320,#7318,#3967,.T.);
#9122=EDGE_CURVE('',#7319,#7321,#3968,.T.);
#9123=EDGE_CURVE('',#7320,#7321,#3969,.T.);
#9124=EDGE_CURVE('',#7322,#7320,#3970,.T.);
#9125=EDGE_CURVE('',#7321,#7323,#3971,.T.);
#9126=EDGE_CURVE('',#7322,#7323,#3972,.T.);
#9127=EDGE_CURVE('',#7324,#7322,#3973,.T.);
#9128=EDGE_CURVE('',#7323,#7325,#3974,.T.);
#9129=EDGE_CURVE('',#7326,#7325,#3975,.T.);
#9130=EDGE_CURVE('',#7324,#7326,#1042,.T.);
#9131=EDGE_CURVE('',#7325,#7316,#3976,.T.);
#9132=EDGE_CURVE('',#7326,#7315,#3977,.T.);
#9133=EDGE_CURVE('',#7327,#7328,#1043,.T.);
#9134=EDGE_CURVE('',#7329,#7327,#3978,.T.);
#9135=EDGE_CURVE('',#7330,#7329,#1044,.T.);
#9136=EDGE_CURVE('',#7328,#7330,#3979,.T.);
#9137=EDGE_CURVE('',#7324,#7331,#3980,.T.);
#9138=EDGE_CURVE('',#7332,#7314,#3981,.T.);
#9139=EDGE_CURVE('',#7333,#7332,#1045,.T.);
#9140=EDGE_CURVE('',#7334,#7333,#3982,.T.);
#9141=EDGE_CURVE('',#7331,#7334,#1046,.T.);
#9142=EDGE_CURVE('',#7279,#7332,#3983,.T.);
#9143=EDGE_CURVE('',#7277,#7327,#3984,.T.);
#9144=EDGE_CURVE('',#7335,#7328,#3985,.T.);
#9145=EDGE_CURVE('',#7336,#7335,#3986,.T.);
#9146=EDGE_CURVE('',#7333,#7336,#3987,.T.);
#9147=EDGE_CURVE('',#7276,#7329,#3988,.T.);
#9148=EDGE_CURVE('',#7274,#7331,#3989,.T.);
#9149=EDGE_CURVE('',#7337,#7334,#3990,.T.);
#9150=EDGE_CURVE('',#7338,#7337,#3991,.T.);
#9151=EDGE_CURVE('',#7330,#7338,#3992,.T.);
#9152=EDGE_CURVE('',#7339,#7340,#1047,.T.);
#9153=EDGE_CURVE('',#7341,#7339,#3993,.T.);
#9154=EDGE_CURVE('',#7342,#7341,#1048,.T.);
#9155=EDGE_CURVE('',#7340,#7342,#3994,.T.);
#9156=EDGE_CURVE('',#7343,#7344,#1049,.T.);
#9157=EDGE_CURVE('',#7345,#7343,#3995,.T.);
#9158=EDGE_CURVE('',#7346,#7345,#1050,.T.);
#9159=EDGE_CURVE('',#7344,#7346,#3996,.T.);
#9160=EDGE_CURVE('',#7347,#7348,#1051,.T.);
#9161=EDGE_CURVE('',#7349,#7347,#3997,.T.);
#9162=EDGE_CURVE('',#7350,#7349,#1052,.T.);
#9163=EDGE_CURVE('',#7348,#7350,#3998,.T.);
#9164=EDGE_CURVE('',#7351,#7352,#1053,.T.);
#9165=EDGE_CURVE('',#7353,#7351,#3999,.T.);
#9166=EDGE_CURVE('',#7354,#7353,#1054,.T.);
#9167=EDGE_CURVE('',#7352,#7354,#4000,.T.);
#9168=EDGE_CURVE('',#7355,#7356,#4001,.T.);
#9169=EDGE_CURVE('',#7356,#7357,#4002,.T.);
#9170=EDGE_CURVE('',#7357,#7358,#4003,.T.);
#9171=EDGE_CURVE('',#7355,#7358,#4004,.T.);
#9172=EDGE_CURVE('',#7359,#7355,#4005,.T.);
#9173=EDGE_CURVE('',#7358,#7360,#4006,.T.);
#9174=EDGE_CURVE('',#7359,#7360,#4007,.T.);
#9175=EDGE_CURVE('',#7361,#7359,#4008,.T.);
#9176=EDGE_CURVE('',#7360,#7362,#4009,.T.);
#9177=EDGE_CURVE('',#7361,#7362,#4010,.T.);
#9178=EDGE_CURVE('',#7363,#7361,#4011,.T.);
#9179=EDGE_CURVE('',#7362,#7364,#4012,.T.);
#9180=EDGE_CURVE('',#7363,#7364,#4013,.T.);
#9181=EDGE_CURVE('',#7365,#7363,#4014,.T.);
#9182=EDGE_CURVE('',#7364,#7366,#4015,.T.);
#9183=EDGE_CURVE('',#7365,#7366,#4016,.T.);
#9184=EDGE_CURVE('',#7367,#7365,#4017,.T.);
#9185=EDGE_CURVE('',#7366,#7368,#4018,.T.);
#9186=EDGE_CURVE('',#7367,#7368,#4019,.T.);
#9187=EDGE_CURVE('',#7369,#7367,#4020,.T.);
#9188=EDGE_CURVE('',#7368,#7370,#4021,.T.);
#9189=EDGE_CURVE('',#7369,#7370,#4022,.T.);
#9190=EDGE_CURVE('',#7371,#7372,#4023,.T.);
#9191=EDGE_CURVE('',#7372,#7373,#4024,.T.);
#9192=EDGE_CURVE('',#7373,#7374,#4025,.T.);
#9193=EDGE_CURVE('',#7371,#7374,#4026,.T.);
#9194=EDGE_CURVE('',#7375,#7376,#4027,.T.);
#9195=EDGE_CURVE('',#7376,#7377,#4028,.T.);
#9196=EDGE_CURVE('',#7377,#7378,#4029,.T.);
#9197=EDGE_CURVE('',#7375,#7378,#4030,.T.);
#9198=EDGE_CURVE('',#7379,#7375,#4031,.T.);
#9199=EDGE_CURVE('',#7378,#7347,#4032,.T.);
#9200=EDGE_CURVE('',#7379,#7348,#4033,.T.);
#9201=EDGE_CURVE('',#7376,#7380,#4034,.T.);
#9202=EDGE_CURVE('',#7380,#7381,#4035,.T.);
#9203=EDGE_CURVE('',#7381,#7377,#4036,.T.);
#9204=EDGE_CURVE('',#7280,#7354,#4037,.T.);
#9205=EDGE_CURVE('',#7285,#7352,#4038,.T.);
#9206=EDGE_CURVE('',#7283,#7343,#4039,.T.);
#9207=EDGE_CURVE('',#7282,#7345,#4040,.T.);
#9208=EDGE_CURVE('',#7382,#7353,#4041,.T.);
#9209=EDGE_CURVE('',#7382,#7383,#4042,.T.);
#9210=EDGE_CURVE('',#7346,#7383,#4043,.T.);
#9211=EDGE_CURVE('',#7291,#7384,#4044,.T.);
#9212=EDGE_CURVE('',#7289,#7339,#4045,.T.);
#9213=EDGE_CURVE('',#7384,#7340,#4046,.T.);
#9214=EDGE_CURVE('',#7288,#7341,#4047,.T.);
#9215=EDGE_CURVE('',#7286,#7385,#4048,.T.);
#9216=EDGE_CURVE('',#7342,#7385,#4049,.T.);
#9217=EDGE_CURVE('',#7384,#7379,#4050,.T.);
#9218=EDGE_CURVE('',#7386,#7350,#4051,.T.);
#9219=EDGE_CURVE('',#7385,#7386,#4052,.T.);
#9220=EDGE_CURVE('',#7387,#7388,#1055,.T.);
#9221=EDGE_CURVE('',#7389,#7387,#4053,.T.);
#9222=EDGE_CURVE('',#7390,#7389,#1056,.T.);
#9223=EDGE_CURVE('',#7388,#7390,#4054,.T.);
#9224=EDGE_CURVE('',#7391,#7392,#1057,.T.);
#9225=EDGE_CURVE('',#7393,#7391,#4055,.T.);
#9226=EDGE_CURVE('',#7394,#7393,#1058,.T.);
#9227=EDGE_CURVE('',#7392,#7394,#4056,.T.);
#9228=EDGE_CURVE('',#7395,#7301,#1059,.T.);
#9229=EDGE_CURVE('',#7396,#7395,#4057,.T.);
#9230=EDGE_CURVE('',#7304,#7396,#1060,.T.);
#9231=EDGE_CURVE('',#7301,#7304,#4058,.T.);
#9232=EDGE_CURVE('',#7302,#7397,#1061,.T.);
#9233=EDGE_CURVE('',#7303,#7302,#4059,.T.);
#9234=EDGE_CURVE('',#7398,#7303,#1062,.T.);
#9235=EDGE_CURVE('',#7397,#7398,#4060,.T.);
#9236=EDGE_CURVE('',#7294,#7390,#4061,.T.);
#9237=EDGE_CURVE('',#7308,#7292,#4062,.T.);
#9238=EDGE_CURVE('',#7393,#7305,#4063,.T.);
#9239=EDGE_CURVE('',#7390,#7393,#4064,.T.);
#9240=EDGE_CURVE('',#7394,#7396,#4065,.T.);
#9241=EDGE_CURVE('',#7392,#7395,#4066,.T.);
#9242=EDGE_CURVE('',#7397,#7387,#4067,.T.);
#9243=EDGE_CURVE('',#7398,#7389,#4068,.T.);
#9244=EDGE_CURVE('',#7307,#7391,#4069,.T.);
#9245=EDGE_CURVE('',#7399,#7306,#4070,.T.);
#9246=EDGE_CURVE('',#7310,#7399,#4071,.T.);
#9247=EDGE_CURVE('',#7400,#7293,#4072,.T.);
#9248=EDGE_CURVE('',#7295,#7400,#4073,.T.);
#9249=EDGE_CURVE('',#7401,#7402,#4074,.T.);
#9250=EDGE_CURVE('',#7402,#7403,#4075,.T.);
#9251=EDGE_CURVE('',#7403,#7404,#4076,.T.);
#9252=EDGE_CURVE('',#7401,#7404,#4077,.T.);
#9253=EDGE_CURVE('',#7404,#7405,#1063,.T.);
#9254=EDGE_CURVE('',#7405,#7373,#4078,.T.);
#9255=EDGE_CURVE('',#7372,#7406,#4079,.T.);
#9256=EDGE_CURVE('',#7406,#7401,#1064,.T.);
#9257=EDGE_CURVE('',#7402,#7311,#1065,.T.);
#9258=EDGE_CURVE('',#7312,#7371,#4080,.T.);
#9259=EDGE_CURVE('',#7374,#7407,#4081,.T.);
#9260=EDGE_CURVE('',#7407,#7403,#1066,.T.);
#9261=EDGE_CURVE('',#7408,#7409,#4082,.T.);
#9262=EDGE_CURVE('',#7409,#7410,#4083,.T.);
#9263=EDGE_CURVE('',#7410,#7411,#4084,.T.);
#9264=EDGE_CURVE('',#7408,#7411,#4085,.T.);
#9265=EDGE_CURVE('',#7411,#7412,#1067,.T.);
#9266=EDGE_CURVE('',#7412,#7357,#4086,.T.);
#9267=EDGE_CURVE('',#7356,#7413,#4087,.T.);
#9268=EDGE_CURVE('',#7413,#7408,#1068,.T.);
#9269=EDGE_CURVE('',#7338,#7414,#4088,.T.);
#9270=EDGE_CURVE('',#7337,#7415,#4089,.T.);
#9271=EDGE_CURVE('',#7415,#7410,#1069,.T.);
#9272=EDGE_CURVE('',#7409,#7414,#1070,.T.);
#9273=EDGE_CURVE('',#7416,#7417,#4090,.T.);
#9274=EDGE_CURVE('',#7417,#7418,#1071,.T.);
#9275=EDGE_CURVE('',#7419,#7418,#4091,.T.);
#9276=EDGE_CURVE('',#7416,#7419,#1072,.T.);
#9277=EDGE_CURVE('',#7420,#7421,#4092,.T.);
#9278=EDGE_CURVE('',#7421,#7417,#4093,.T.);
#9279=EDGE_CURVE('',#7420,#7416,#4094,.T.);
#9280=EDGE_CURVE('',#7422,#7423,#4095,.T.);
#9281=EDGE_CURVE('',#7423,#7421,#1073,.T.);
#9282=EDGE_CURVE('',#7422,#7420,#1074,.T.);
#9283=EDGE_CURVE('',#7418,#7423,#4096,.T.);
#9284=EDGE_CURVE('',#7419,#7422,#4097,.T.);
#9285=EDGE_CURVE('',#7424,#7425,#4098,.T.);
#9286=EDGE_CURVE('',#7425,#7426,#1075,.T.);
#9287=EDGE_CURVE('',#7427,#7426,#4099,.T.);
#9288=EDGE_CURVE('',#7424,#7427,#1076,.T.);
#9289=EDGE_CURVE('',#7428,#7429,#4100,.T.);
#9290=EDGE_CURVE('',#7429,#7425,#4101,.T.);
#9291=EDGE_CURVE('',#7428,#7424,#4102,.T.);
#9292=EDGE_CURVE('',#7430,#7431,#4103,.T.);
#9293=EDGE_CURVE('',#7431,#7429,#1077,.T.);
#9294=EDGE_CURVE('',#7430,#7428,#1078,.T.);
#9295=EDGE_CURVE('',#7426,#7431,#4104,.T.);
#9296=EDGE_CURVE('',#7427,#7430,#4105,.T.);
#9297=EDGE_CURVE('',#7432,#7433,#1079,.T.);
#9298=EDGE_CURVE('',#7433,#7434,#4106,.T.);
#9299=EDGE_CURVE('',#7435,#7434,#4107,.T.);
#9300=EDGE_CURVE('',#7436,#7435,#4108,.T.);
#9301=EDGE_CURVE('',#7432,#7436,#4109,.T.);
#9302=EDGE_CURVE('',#7349,#7432,#4110,.T.);
#9303=EDGE_CURVE('',#7436,#7437,#4111,.T.);
#9304=EDGE_CURVE('',#7437,#7386,#4112,.T.);
#9305=EDGE_CURVE('',#7386,#7438,#4113,.T.);
#9306=EDGE_CURVE('',#7437,#7438,#1080,.T.);
#9307=EDGE_CURVE('',#7439,#7435,#4114,.T.);
#9308=EDGE_CURVE('',#7439,#7440,#4115,.T.);
#9309=EDGE_CURVE('',#7440,#7436,#4116,.T.);
#9310=EDGE_CURVE('',#7406,#7414,#4117,.T.);
#9311=EDGE_CURVE('',#7413,#7438,#4118,.T.);
#9312=EDGE_CURVE('',#7440,#7309,#1081,.T.);
#9313=EDGE_CURVE('',#7292,#7441,#4119,.T.);
#9314=EDGE_CURVE('',#7441,#7344,#4120,.T.);
#9315=EDGE_CURVE('',#7380,#7383,#4121,.T.);
#9316=EDGE_CURVE('',#7335,#7369,#4122,.T.);
#9317=EDGE_CURVE('',#7441,#7442,#4123,.T.);
#9318=EDGE_CURVE('',#7442,#7351,#4124,.T.);
#9319=EDGE_CURVE('',#7370,#7336,#4125,.T.);
#9320=EDGE_CURVE('',#7412,#7432,#4126,.T.);
#9321=EDGE_CURVE('',#7382,#7381,#4127,.T.);
#9322=EDGE_CURVE('',#7442,#7400,#4128,.T.);
#9323=EDGE_CURVE('',#7388,#7298,#4129,.T.);
#9324=EDGE_CURVE('',#7399,#7407,#4130,.T.);
#9325=EDGE_CURVE('',#7405,#7415,#4131,.T.);
#9326=EDGE_CURVE('',#7411,#7433,#4132,.T.);
#9327=EDGE_CURVE('',#7404,#7410,#4133,.T.);
#9328=EDGE_CURVE('',#7443,#7403,#4134,.T.);
#9329=EDGE_CURVE('',#7443,#7444,#4135,.T.);
#9330=EDGE_CURVE('',#7444,#7434,#4136,.T.);
#9331=EDGE_CURVE('',#7444,#7439,#4137,.T.);
#9332=EDGE_CURVE('',#7399,#7443,#1082,.T.);
#9333=EDGE_CURVE('',#7445,#7446,#1083,.T.);
#9334=EDGE_CURVE('',#7447,#7446,#1084,.T.);
#9335=EDGE_CURVE('',#7447,#7445,#1085,.T.);
#9336=EDGE_CURVE('',#7448,#7449,#1086,.T.);
#9337=EDGE_CURVE('',#7448,#7450,#1087,.T.);
#9338=EDGE_CURVE('',#7450,#7449,#1088,.T.);
#9339=EDGE_CURVE('',#7451,#7452,#1089,.T.);
#9340=EDGE_CURVE('',#7452,#7453,#1090,.T.);
#9341=EDGE_CURVE('',#7454,#7453,#1091,.T.);
#9342=EDGE_CURVE('',#7454,#7451,#236,.T.);
#9343=EDGE_CURVE('',#7455,#7456,#1092,.T.);
#9344=EDGE_CURVE('',#7456,#7457,#1093,.T.);
#9345=EDGE_CURVE('',#7455,#7457,#1094,.T.);
#9346=EDGE_CURVE('',#7458,#7459,#1095,.T.);
#9347=EDGE_CURVE('',#7458,#7460,#1096,.T.);
#9348=EDGE_CURVE('',#7460,#7461,#1097,.T.);
#9349=EDGE_CURVE('',#7461,#7459,#237,.T.);
#9350=EDGE_CURVE('',#7462,#7463,#1098,.T.);
#9351=EDGE_CURVE('',#7462,#7464,#1099,.T.);
#9352=EDGE_CURVE('',#7464,#7463,#1100,.T.);
#9353=EDGE_CURVE('',#7465,#7466,#1101,.T.);
#9354=EDGE_CURVE('',#7466,#7467,#1102,.T.);
#9355=EDGE_CURVE('',#7467,#7468,#238,.T.);
#9356=EDGE_CURVE('',#7465,#7468,#1103,.T.);
#9357=EDGE_CURVE('',#7469,#7470,#1104,.T.);
#9358=EDGE_CURVE('',#7469,#7471,#239,.T.);
#9359=EDGE_CURVE('',#7471,#7472,#1105,.T.);
#9360=EDGE_CURVE('',#7472,#7470,#1106,.T.);
#9361=EDGE_CURVE('',#7473,#7474,#1107,.T.);
#9362=EDGE_CURVE('',#7474,#7475,#1108,.T.);
#9363=EDGE_CURVE('',#7473,#7475,#1109,.T.);
#9364=EDGE_CURVE('',#7476,#7477,#1110,.T.);
#9365=EDGE_CURVE('',#7478,#7477,#1111,.T.);
#9366=EDGE_CURVE('',#7478,#7476,#1112,.T.);
#9367=EDGE_CURVE('',#7479,#7479,#1113,.T.);
#9368=EDGE_CURVE('',#7479,#7480,#1114,.T.);
#9369=EDGE_CURVE('',#7480,#7480,#1115,.T.);
#9370=EDGE_CURVE('',#7481,#7482,#1116,.T.);
#9371=EDGE_CURVE('',#7482,#7481,#1117,.T.);
#9372=EDGE_CURVE('',#7482,#7483,#1118,.T.);
#9373=EDGE_CURVE('',#7483,#7483,#1119,.T.);
#9374=EDGE_CURVE('',#7484,#7484,#1120,.T.);
#9375=EDGE_CURVE('',#7484,#7485,#1121,.T.);
#9376=EDGE_CURVE('',#7486,#7485,#1122,.T.);
#9377=EDGE_CURVE('',#7485,#7486,#1123,.T.);
#9378=EDGE_CURVE('',#7487,#7487,#1124,.T.);
#9379=EDGE_CURVE('',#7487,#7488,#1125,.T.);
#9380=EDGE_CURVE('',#7488,#7488,#1126,.T.);
#9381=EDGE_CURVE('',#7489,#7489,#1127,.T.);
#9382=EDGE_CURVE('',#7489,#7490,#1128,.T.);
#9383=EDGE_CURVE('',#7491,#7490,#1129,.T.);
#9384=EDGE_CURVE('',#7490,#7491,#1130,.T.);
#9385=EDGE_CURVE('',#7492,#7492,#1131,.T.);
#9386=EDGE_CURVE('',#7492,#7493,#1132,.T.);
#9387=EDGE_CURVE('',#7493,#7493,#1133,.T.);
#9388=EDGE_CURVE('',#7494,#7494,#1134,.T.);
#9389=EDGE_CURVE('',#7494,#7495,#1135,.T.);
#9390=EDGE_CURVE('',#7495,#7495,#1136,.T.);
#9391=EDGE_CURVE('',#7496,#7496,#1137,.T.);
#9392=EDGE_CURVE('',#7496,#7497,#1138,.T.);
#9393=EDGE_CURVE('',#7497,#7497,#1139,.T.);
#9394=EDGE_CURVE('',#7498,#7498,#1140,.T.);
#9395=EDGE_CURVE('',#7498,#7499,#1141,.T.);
#9396=EDGE_CURVE('',#7499,#7499,#1142,.T.);
#9397=EDGE_CURVE('',#7481,#7492,#4138,.T.);
#9398=EDGE_CURVE('',#7495,#7500,#4139,.T.);
#9399=EDGE_CURVE('',#7501,#7500,#1143,.T.);
#9400=EDGE_CURVE('',#7502,#7501,#240,.T.);
#9401=EDGE_CURVE('',#7503,#7502,#241,.T.);
#9402=EDGE_CURVE('',#7503,#7504,#1144,.T.);
#9403=EDGE_CURVE('',#7468,#7504,#242,.T.);
#9404=EDGE_CURVE('',#7459,#7467,#1145,.T.);
#9405=EDGE_CURVE('',#7505,#7461,#243,.T.);
#9406=EDGE_CURVE('',#7505,#7506,#1146,.T.);
#9407=EDGE_CURVE('',#7507,#7506,#244,.T.);
#9408=EDGE_CURVE('',#7508,#7507,#245,.T.);
#9409=EDGE_CURVE('',#7509,#7508,#1147,.T.);
#9410=EDGE_CURVE('',#7510,#7509,#246,.T.);
#9411=EDGE_CURVE('',#7511,#7510,#247,.T.);
#9412=EDGE_CURVE('',#7511,#7512,#1148,.T.);
#9413=EDGE_CURVE('',#7451,#7512,#248,.T.);
#9414=EDGE_CURVE('',#7513,#7454,#1149,.T.);
#9415=EDGE_CURVE('',#7514,#7513,#249,.T.);
#9416=EDGE_CURVE('',#7515,#7514,#250,.T.);
#9417=EDGE_CURVE('',#7515,#7516,#1150,.T.);
#9418=EDGE_CURVE('',#7517,#7516,#251,.T.);
#9419=EDGE_CURVE('',#7518,#7517,#252,.T.);
#9420=EDGE_CURVE('',#7471,#7518,#1151,.T.);
#9421=EDGE_CURVE('',#7519,#7469,#253,.T.);
#9422=EDGE_CURVE('',#7519,#7520,#1152,.T.);
#9423=EDGE_CURVE('',#7521,#7520,#254,.T.);
#9424=EDGE_CURVE('',#7522,#7521,#255,.T.);
#9425=EDGE_CURVE('',#7500,#7522,#1153,.T.);
#9426=EDGE_CURVE('',#7523,#7524,#1154,.T.);
#9427=EDGE_CURVE('',#7506,#7524,#256,.T.);
#9428=EDGE_CURVE('',#7525,#7505,#257,.T.);
#9429=EDGE_CURVE('',#7525,#7526,#1155,.T.);
#9430=EDGE_CURVE('',#7504,#7526,#258,.T.);
#9431=EDGE_CURVE('',#7527,#7503,#259,.T.);
#9432=EDGE_CURVE('',#7527,#7528,#1156,.T.);
#9433=EDGE_CURVE('',#7528,#7529,#1157,.T.);
#9434=EDGE_CURVE('',#7529,#7496,#4140,.T.);
#9435=EDGE_CURVE('',#7529,#7530,#1158,.T.);
#9436=EDGE_CURVE('',#7520,#7530,#260,.T.);
#9437=EDGE_CURVE('',#7531,#7519,#261,.T.);
#9438=EDGE_CURVE('',#7531,#7532,#1159,.T.);
#9439=EDGE_CURVE('',#7516,#7532,#262,.T.);
#9440=EDGE_CURVE('',#7533,#7515,#263,.T.);
#9441=EDGE_CURVE('',#7533,#7534,#1160,.T.);
#9442=EDGE_CURVE('',#7512,#7534,#264,.T.);
#9443=EDGE_CURVE('',#7523,#7511,#265,.T.);
#9444=EDGE_CURVE('',#7499,#7479,#4141,.T.);
#9445=EDGE_CURVE('',#7488,#7491,#4142,.T.);
#9446=EDGE_CURVE('',#7535,#7535,#1161,.T.);
#9447=EDGE_CURVE('',#7535,#7484,#4143,.T.);
#9448=EDGE_CURVE('',#7483,#7486,#4144,.T.);
#9449=EDGE_CURVE('',#7536,#7537,#1162,.T.);
#9450=EDGE_CURVE('',#7537,#7536,#1163,.T.);
#9451=EDGE_CURVE('',#7537,#7538,#1164,.T.);
#9452=EDGE_CURVE('',#7538,#7538,#1165,.T.);
#9453=EDGE_CURVE('',#7539,#7539,#1166,.T.);
#9454=EDGE_CURVE('',#7539,#7540,#1167,.T.);
#9455=EDGE_CURVE('',#7540,#7540,#1168,.T.);
#9456=EDGE_CURVE('',#7541,#7542,#1169,.T.);
#9457=EDGE_CURVE('',#7542,#7541,#1170,.T.);
#9458=EDGE_CURVE('',#7542,#7543,#1171,.T.);
#9459=EDGE_CURVE('',#7543,#7543,#1172,.T.);
#9460=EDGE_CURVE('',#7544,#7477,#4145,.T.);
#9461=EDGE_CURVE('',#7544,#7545,#1173,.T.);
#9462=EDGE_CURVE('',#7478,#7545,#4146,.T.);
#9463=EDGE_CURVE('',#7521,#7545,#1174,.T.);
#9464=EDGE_CURVE('',#7544,#7522,#1175,.T.);
#9465=EDGE_CURVE('',#7546,#7544,#1176,.T.);
#9466=EDGE_CURVE('',#7546,#7501,#1177,.T.);
#9467=EDGE_CURVE('',#7547,#7530,#4147,.T.);
#9468=EDGE_CURVE('',#7547,#7548,#266,.T.);
#9469=EDGE_CURVE('',#7549,#7548,#4148,.T.);
#9470=EDGE_CURVE('',#7545,#7549,#4149,.T.);
#9471=EDGE_CURVE('',#7550,#7551,#267,.T.);
#9472=EDGE_CURVE('',#7476,#7551,#4150,.T.);
#9473=EDGE_CURVE('',#7552,#7478,#4151,.T.);
#9474=EDGE_CURVE('',#7550,#7552,#1178,.T.);
#9475=EDGE_CURVE('',#7477,#7475,#1179,.T.);
#9476=EDGE_CURVE('',#7473,#7476,#1180,.T.);
#9477=EDGE_CURVE('',#7553,#7502,#1181,.T.);
#9478=EDGE_CURVE('',#7546,#7553,#1182,.T.);
#9479=EDGE_CURVE('',#7554,#7555,#268,.T.);
#9480=EDGE_CURVE('',#7548,#7555,#1183,.T.);
#9481=EDGE_CURVE('',#7554,#7547,#1184,.T.);
#9482=EDGE_CURVE('',#7556,#7557,#269,.T.);
#9483=EDGE_CURVE('',#7551,#7557,#1185,.T.);
#9484=EDGE_CURVE('',#7556,#7550,#1186,.T.);
#9485=EDGE_CURVE('',#7553,#7474,#4152,.T.);
#9486=EDGE_CURVE('',#7475,#7546,#4153,.T.);
#9487=EDGE_CURVE('',#7558,#7553,#4154,.T.);
#9488=EDGE_CURVE('',#7559,#7558,#4155,.T.);
#9489=EDGE_CURVE('',#7559,#7560,#270,.T.);
#9490=EDGE_CURVE('',#7527,#7560,#4156,.T.);
#9491=EDGE_CURVE('',#7531,#7554,#4157,.T.);
#9492=EDGE_CURVE('',#7561,#7470,#4158,.T.);
#9493=EDGE_CURVE('',#7555,#7561,#4159,.T.);
#9494=EDGE_CURVE('',#7562,#7563,#1187,.T.);
#9495=EDGE_CURVE('',#7557,#7563,#4160,.T.);
#9496=EDGE_CURVE('',#7564,#7556,#1188,.T.);
#9497=EDGE_CURVE('',#7562,#7564,#4161,.T.);
#9498=EDGE_CURVE('',#7565,#7566,#1189,.T.);
#9499=EDGE_CURVE('',#7474,#7565,#4162,.T.);
#9500=EDGE_CURVE('',#7567,#7473,#4163,.T.);
#9501=EDGE_CURVE('',#7567,#7566,#271,.T.);
#9502=EDGE_CURVE('',#7568,#7569,#272,.T.);
#9503=EDGE_CURVE('',#7560,#7569,#1190,.T.);
#9504=EDGE_CURVE('',#7568,#7559,#1191,.T.);
#9505=EDGE_CURVE('',#7570,#7563,#1192,.T.);
#9506=EDGE_CURVE('',#7562,#7570,#1193,.T.);
#9507=EDGE_CURVE('',#7566,#7571,#1194,.T.);
#9508=EDGE_CURVE('',#7572,#7567,#1195,.T.);
#9509=EDGE_CURVE('',#7572,#7571,#273,.T.);
#9510=EDGE_CURVE('',#7569,#7526,#4164,.T.);
#9511=EDGE_CURVE('',#7573,#7568,#4165,.T.);
#9512=EDGE_CURVE('',#7465,#7573,#4166,.T.);
#9513=EDGE_CURVE('',#7518,#7574,#1196,.T.);
#9514=EDGE_CURVE('',#7472,#7574,#1197,.T.);
#9515=EDGE_CURVE('',#7570,#7472,#4167,.T.);
#9516=EDGE_CURVE('',#7470,#7562,#4168,.T.);
#9517=EDGE_CURVE('',#7563,#7463,#1198,.T.);
#9518=EDGE_CURVE('',#7462,#7570,#1199,.T.);
#9519=EDGE_CURVE('',#7575,#7576,#1200,.T.);
#9520=EDGE_CURVE('',#7577,#7576,#4169,.T.);
#9521=EDGE_CURVE('',#7571,#7577,#1201,.T.);
#9522=EDGE_CURVE('',#7575,#7572,#4170,.T.);
#9523=EDGE_CURVE('',#7517,#7578,#1202,.T.);
#9524=EDGE_CURVE('',#7578,#7574,#1203,.T.);
#9525=EDGE_CURVE('',#7579,#7576,#1204,.T.);
#9526=EDGE_CURVE('',#7575,#7579,#1205,.T.);
#9527=EDGE_CURVE('',#7466,#7579,#4171,.T.);
#9528=EDGE_CURVE('',#7576,#7465,#4172,.T.);
#9529=EDGE_CURVE('',#7458,#7466,#1206,.T.);
#9530=EDGE_CURVE('',#7580,#7532,#4173,.T.);
#9531=EDGE_CURVE('',#7580,#7581,#274,.T.);
#9532=EDGE_CURVE('',#7582,#7581,#4174,.T.);
#9533=EDGE_CURVE('',#7578,#7582,#4175,.T.);
#9534=EDGE_CURVE('',#7464,#7578,#4176,.T.);
#9535=EDGE_CURVE('',#7574,#7462,#4177,.T.);
#9536=EDGE_CURVE('',#7583,#7584,#275,.T.);
#9537=EDGE_CURVE('',#7463,#7584,#4178,.T.);
#9538=EDGE_CURVE('',#7585,#7464,#4179,.T.);
#9539=EDGE_CURVE('',#7583,#7585,#1207,.T.);
#9540=EDGE_CURVE('',#7586,#7587,#1208,.T.);
#9541=EDGE_CURVE('',#7579,#7587,#1209,.T.);
#9542=EDGE_CURVE('',#7586,#7575,#1210,.T.);
#9543=EDGE_CURVE('',#7588,#7589,#276,.T.);
#9544=EDGE_CURVE('',#7581,#7589,#1211,.T.);
#9545=EDGE_CURVE('',#7588,#7580,#1212,.T.);
#9546=EDGE_CURVE('',#7590,#7591,#277,.T.);
#9547=EDGE_CURVE('',#7584,#7591,#1213,.T.);
#9548=EDGE_CURVE('',#7590,#7583,#1214,.T.);
#9549=EDGE_CURVE('',#7586,#7592,#1215,.T.);
#9550=EDGE_CURVE('',#7592,#7587,#1216,.T.);
#9551=EDGE_CURVE('',#7460,#7592,#4180,.T.);
#9552=EDGE_CURVE('',#7587,#7458,#4181,.T.);
#9553=EDGE_CURVE('',#7593,#7460,#4182,.T.);
#9554=EDGE_CURVE('',#7594,#7593,#4183,.T.);
#9555=EDGE_CURVE('',#7594,#7595,#278,.T.);
#9556=EDGE_CURVE('',#7525,#7595,#4184,.T.);
#9557=EDGE_CURVE('',#7533,#7588,#4185,.T.);
#9558=EDGE_CURVE('',#7514,#7596,#1217,.T.);
#9559=EDGE_CURVE('',#7597,#7596,#4186,.T.);
#9560=EDGE_CURVE('',#7589,#7597,#4187,.T.);
#9561=EDGE_CURVE('',#7591,#7457,#4188,.T.);
#9562=EDGE_CURVE('',#7598,#7590,#1218,.T.);
#9563=EDGE_CURVE('',#7455,#7598,#4189,.T.);
#9564=EDGE_CURVE('',#7599,#7600,#1219,.T.);
#9565=EDGE_CURVE('',#7592,#7599,#4190,.T.);
#9566=EDGE_CURVE('',#7601,#7586,#4191,.T.);
#9567=EDGE_CURVE('',#7601,#7600,#279,.T.);
#9568=EDGE_CURVE('',#7602,#7603,#280,.T.);
#9569=EDGE_CURVE('',#7595,#7603,#1220,.T.);
#9570=EDGE_CURVE('',#7602,#7594,#1221,.T.);
#9571=EDGE_CURVE('',#7513,#7604,#1222,.T.);
#9572=EDGE_CURVE('',#7604,#7596,#1223,.T.);
#9573=EDGE_CURVE('',#7600,#7605,#1224,.T.);
#9574=EDGE_CURVE('',#7606,#7601,#1225,.T.);
#9575=EDGE_CURVE('',#7606,#7605,#281,.T.);
#9576=EDGE_CURVE('',#7607,#7507,#1226,.T.);
#9577=EDGE_CURVE('',#7603,#7524,#4192,.T.);
#9578=EDGE_CURVE('',#7608,#7602,#4193,.T.);
#9579=EDGE_CURVE('',#7607,#7608,#4194,.T.);
#9580=EDGE_CURVE('',#7604,#7453,#1227,.T.);
#9581=EDGE_CURVE('',#7456,#7604,#4195,.T.);
#9582=EDGE_CURVE('',#7596,#7455,#4196,.T.);
#9583=EDGE_CURVE('',#7609,#7610,#1228,.T.);
#9584=EDGE_CURVE('',#7457,#7610,#1229,.T.);
#9585=EDGE_CURVE('',#7609,#7456,#1230,.T.);
#9586=EDGE_CURVE('',#7611,#7449,#4197,.T.);
#9587=EDGE_CURVE('',#7605,#7611,#1231,.T.);
#9588=EDGE_CURVE('',#7448,#7606,#4198,.T.);
#9589=EDGE_CURVE('',#7612,#7508,#1232,.T.);
#9590=EDGE_CURVE('',#7607,#7612,#1233,.T.);
#9591=EDGE_CURVE('',#7613,#7610,#1234,.T.);
#9592=EDGE_CURVE('',#7609,#7613,#1235,.T.);
#9593=EDGE_CURVE('',#7612,#7450,#4199,.T.);
#9594=EDGE_CURVE('',#7449,#7607,#4200,.T.);
#9595=EDGE_CURVE('',#7614,#7612,#1236,.T.);
#9596=EDGE_CURVE('',#7614,#7509,#1237,.T.);
#9597=EDGE_CURVE('',#7615,#7534,#4201,.T.);
#9598=EDGE_CURVE('',#7615,#7616,#282,.T.);
#9599=EDGE_CURVE('',#7617,#7616,#4202,.T.);
#9600=EDGE_CURVE('',#7452,#7617,#4203,.T.);
#9601=EDGE_CURVE('',#7613,#7452,#4204,.T.);
#9602=EDGE_CURVE('',#7453,#7609,#4205,.T.);
#9603=EDGE_CURVE('',#7618,#7619,#283,.T.);
#9604=EDGE_CURVE('',#7610,#7619,#4206,.T.);
#9605=EDGE_CURVE('',#7620,#7613,#4207,.T.);
#9606=EDGE_CURVE('',#7618,#7620,#1238,.T.);
#9607=EDGE_CURVE('',#7450,#7446,#1239,.T.);
#9608=EDGE_CURVE('',#7621,#7448,#1240,.T.);
#9609=EDGE_CURVE('',#7447,#7621,#1241,.T.);
#9610=EDGE_CURVE('',#7614,#7622,#1242,.T.);
#9611=EDGE_CURVE('',#7622,#7510,#1243,.T.);
#9612=EDGE_CURVE('',#7623,#7624,#284,.T.);
#9613=EDGE_CURVE('',#7616,#7624,#1244,.T.);
#9614=EDGE_CURVE('',#7623,#7615,#1245,.T.);
#9615=EDGE_CURVE('',#7625,#7626,#285,.T.);
#9616=EDGE_CURVE('',#7619,#7626,#1246,.T.);
#9617=EDGE_CURVE('',#7625,#7618,#1247,.T.);
#9618=EDGE_CURVE('',#7622,#7445,#4208,.T.);
#9619=EDGE_CURVE('',#7446,#7614,#4209,.T.);
#9620=EDGE_CURVE('',#7523,#7623,#4210,.T.);
#9621=EDGE_CURVE('',#7627,#7622,#4211,.T.);
#9622=EDGE_CURVE('',#7624,#7627,#4212,.T.);
#9623=EDGE_CURVE('',#7628,#7625,#1248,.T.);
#9624=EDGE_CURVE('',#7445,#7628,#4213,.T.);
#9625=EDGE_CURVE('',#7626,#7447,#4214,.T.);
#9626=EDGE_CURVE('',#7629,#7629,#1249,.T.);
#9627=EDGE_CURVE('',#7629,#7630,#1250,.T.);
#9628=EDGE_CURVE('',#7630,#7630,#1251,.T.);
#9629=EDGE_CURVE('',#7585,#7582,#4215,.T.);
#9630=EDGE_CURVE('',#7597,#7598,#4216,.T.);
#9631=EDGE_CURVE('',#7620,#7617,#4217,.T.);
#9632=EDGE_CURVE('',#7627,#7628,#4218,.T.);
#9633=EDGE_CURVE('',#7611,#7608,#4219,.T.);
#9634=EDGE_CURVE('',#7593,#7599,#4220,.T.);
#9635=EDGE_CURVE('',#7577,#7573,#4221,.T.);
#9636=EDGE_CURVE('',#7558,#7565,#4222,.T.);
#9637=EDGE_CURVE('',#7552,#7549,#4223,.T.);
#9638=EDGE_CURVE('',#7561,#7564,#4224,.T.);
#9639=EDGE_CURVE('',#7631,#7631,#1252,.T.);
#9640=EDGE_CURVE('',#7632,#7632,#1253,.T.);
#9641=EDGE_CURVE('',#7632,#7631,#1254,.T.);
#9642=EDGE_CURVE('',#7541,#7632,#4225,.T.);
#9643=EDGE_CURVE('',#7543,#7528,#4226,.T.);
#9644=EDGE_CURVE('',#7540,#7621,#4227,.T.);
#9645=EDGE_CURVE('',#7536,#7629,#4228,.T.);
#9646=EDGE_CURVE('',#7633,#7634,#1255,.T.);
#9647=EDGE_CURVE('',#7635,#7633,#4229,.T.);
#9648=EDGE_CURVE('',#7636,#7635,#1256,.T.);
#9649=EDGE_CURVE('',#7634,#7636,#4230,.T.);
#9650=EDGE_CURVE('',#7637,#7638,#1257,.T.);
#9651=EDGE_CURVE('',#7639,#7637,#4231,.T.);
#9652=EDGE_CURVE('',#7640,#7639,#1258,.T.);
#9653=EDGE_CURVE('',#7638,#7640,#4232,.T.);
#9654=EDGE_CURVE('',#7641,#7642,#1259,.T.);
#9655=EDGE_CURVE('',#7643,#7641,#4233,.T.);
#9656=EDGE_CURVE('',#7644,#7643,#1260,.T.);
#9657=EDGE_CURVE('',#7642,#7644,#4234,.T.);
#9658=EDGE_CURVE('',#7645,#7646,#1261,.T.);
#9659=EDGE_CURVE('',#7647,#7645,#4235,.T.);
#9660=EDGE_CURVE('',#7648,#7647,#1262,.T.);
#9661=EDGE_CURVE('',#7646,#7648,#4236,.T.);
#9662=EDGE_CURVE('',#7649,#7650,#1263,.T.);
#9663=EDGE_CURVE('',#7651,#7649,#4237,.T.);
#9664=EDGE_CURVE('',#7652,#7651,#1264,.T.);
#9665=EDGE_CURVE('',#7650,#7652,#4238,.T.);
#9666=EDGE_CURVE('',#7653,#7654,#1265,.T.);
#9667=EDGE_CURVE('',#7655,#7653,#4239,.T.);
#9668=EDGE_CURVE('',#7656,#7655,#1266,.T.);
#9669=EDGE_CURVE('',#7654,#7656,#4240,.T.);
#9670=EDGE_CURVE('',#7657,#7658,#1267,.T.);
#9671=EDGE_CURVE('',#7658,#7657,#1268,.T.);
#9672=EDGE_CURVE('',#7658,#7659,#4241,.T.);
#9673=EDGE_CURVE('',#7659,#7659,#1269,.T.);
#9674=EDGE_CURVE('',#7660,#7661,#1270,.T.);
#9675=EDGE_CURVE('',#7661,#7660,#1271,.T.);
#9676=EDGE_CURVE('',#7661,#7662,#4242,.T.);
#9677=EDGE_CURVE('',#7662,#7662,#1272,.T.);
#9678=EDGE_CURVE('',#7663,#7664,#1273,.T.);
#9679=EDGE_CURVE('',#7664,#7663,#1274,.T.);
#9680=EDGE_CURVE('',#7664,#7665,#4243,.T.);
#9681=EDGE_CURVE('',#7665,#7665,#1275,.T.);
#9682=EDGE_CURVE('',#7666,#7667,#1276,.T.);
#9683=EDGE_CURVE('',#7667,#7666,#1277,.T.);
#9684=EDGE_CURVE('',#7667,#7668,#4244,.T.);
#9685=EDGE_CURVE('',#7668,#7668,#1278,.T.);
#9686=EDGE_CURVE('',#7669,#7670,#1279,.T.);
#9687=EDGE_CURVE('',#7670,#7669,#1280,.T.);
#9688=EDGE_CURVE('',#7670,#7671,#4245,.T.);
#9689=EDGE_CURVE('',#7671,#7671,#1281,.T.);
#9690=EDGE_CURVE('',#7672,#7673,#1282,.T.);
#9691=EDGE_CURVE('',#7673,#7672,#1283,.T.);
#9692=EDGE_CURVE('',#7673,#7674,#4246,.T.);
#9693=EDGE_CURVE('',#7674,#7674,#1284,.T.);
#9694=EDGE_CURVE('',#7675,#7676,#1285,.T.);
#9695=EDGE_CURVE('',#7676,#7675,#1286,.T.);
#9696=EDGE_CURVE('',#7676,#7677,#4247,.T.);
#9697=EDGE_CURVE('',#7677,#7677,#1287,.T.);
#9698=EDGE_CURVE('',#7678,#7679,#1288,.T.);
#9699=EDGE_CURVE('',#7679,#7678,#1289,.T.);
#9700=EDGE_CURVE('',#7679,#7680,#4248,.T.);
#9701=EDGE_CURVE('',#7680,#7680,#1290,.T.);
#9702=EDGE_CURVE('',#7681,#7682,#1291,.T.);
#9703=EDGE_CURVE('',#7682,#7681,#1292,.T.);
#9704=EDGE_CURVE('',#7682,#7683,#4249,.T.);
#9705=EDGE_CURVE('',#7683,#7683,#1293,.T.);
#9706=EDGE_CURVE('',#7684,#7685,#1294,.T.);
#9707=EDGE_CURVE('',#7685,#7684,#1295,.T.);
#9708=EDGE_CURVE('',#7685,#7686,#4250,.T.);
#9709=EDGE_CURVE('',#7686,#7686,#1296,.T.);
#9710=EDGE_CURVE('',#7687,#7688,#1297,.T.);
#9711=EDGE_CURVE('',#7688,#7687,#1298,.T.);
#9712=EDGE_CURVE('',#7688,#7689,#4251,.T.);
#9713=EDGE_CURVE('',#7689,#7689,#1299,.T.);
#9714=EDGE_CURVE('',#7690,#7691,#1300,.T.);
#9715=EDGE_CURVE('',#7691,#7690,#1301,.T.);
#9716=EDGE_CURVE('',#7691,#7692,#4252,.T.);
#9717=EDGE_CURVE('',#7692,#7692,#1302,.T.);
#9718=EDGE_CURVE('',#7693,#7694,#1303,.T.);
#9719=EDGE_CURVE('',#7694,#7693,#1304,.T.);
#9720=EDGE_CURVE('',#7694,#7695,#4253,.T.);
#9721=EDGE_CURVE('',#7695,#7695,#1305,.T.);
#9722=EDGE_CURVE('',#7696,#7697,#4254,.T.);
#9723=EDGE_CURVE('',#7697,#7698,#4255,.T.);
#9724=EDGE_CURVE('',#7698,#7699,#4256,.T.);
#9725=EDGE_CURVE('',#7699,#7696,#4257,.T.);
#9726=EDGE_CURVE('',#7700,#7701,#1306,.T.);
#9727=EDGE_CURVE('',#7702,#7701,#4258,.T.);
#9728=EDGE_CURVE('',#7703,#7702,#4259,.T.);
#9729=EDGE_CURVE('',#7704,#7703,#1307,.T.);
#9730=EDGE_CURVE('',#7705,#7704,#4260,.T.);
#9731=EDGE_CURVE('',#7706,#7705,#1308,.T.);
#9732=EDGE_CURVE('',#7706,#7707,#4261,.T.);
#9733=EDGE_CURVE('',#7707,#7708,#4262,.T.);
#9734=EDGE_CURVE('',#7708,#7700,#4263,.T.);
#9735=EDGE_CURVE('',#7709,#7710,#4264,.T.);
#9736=EDGE_CURVE('',#7710,#7711,#4265,.T.);
#9737=EDGE_CURVE('',#7711,#7712,#4266,.T.);
#9738=EDGE_CURVE('',#7712,#7709,#4267,.T.);
#9739=EDGE_CURVE('',#7713,#7714,#4268,.T.);
#9740=EDGE_CURVE('',#7711,#7714,#4269,.T.);
#9741=EDGE_CURVE('',#7715,#7710,#4270,.T.);
#9742=EDGE_CURVE('',#7715,#7713,#4271,.T.);
#9743=EDGE_CURVE('',#7714,#7716,#4272,.T.);
#9744=EDGE_CURVE('',#7712,#7716,#4273,.T.);
#9745=EDGE_CURVE('',#7716,#7717,#4274,.T.);
#9746=EDGE_CURVE('',#7718,#7717,#4275,.T.);
#9747=EDGE_CURVE('',#7709,#7718,#4276,.T.);
#9748=EDGE_CURVE('',#7704,#7719,#4277,.T.);
#9749=EDGE_CURVE('',#7720,#7703,#4278,.T.);
#9750=EDGE_CURVE('',#7719,#7720,#1309,.T.);
#9751=EDGE_CURVE('',#7706,#7709,#4279,.T.);
#9752=EDGE_CURVE('',#7721,#7705,#4280,.T.);
#9753=EDGE_CURVE('',#7722,#7721,#1310,.T.);
#9754=EDGE_CURVE('',#7710,#7722,#4281,.T.);
#9755=EDGE_CURVE('',#7723,#7724,#1311,.T.);
#9756=EDGE_CURVE('',#7725,#7723,#4282,.T.);
#9757=EDGE_CURVE('',#7726,#7725,#1312,.T.);
#9758=EDGE_CURVE('',#7724,#7726,#4283,.T.);
#9759=EDGE_CURVE('',#7716,#7700,#4284,.T.);
#9760=EDGE_CURVE('',#7727,#7714,#4285,.T.);
#9761=EDGE_CURVE('',#7728,#7727,#1313,.T.);
#9762=EDGE_CURVE('',#7701,#7728,#4286,.T.);
#9763=EDGE_CURVE('',#7728,#7729,#4287,.T.);
#9764=EDGE_CURVE('',#7730,#7727,#4288,.T.);
#9765=EDGE_CURVE('',#7731,#7730,#4289,.T.);
#9766=EDGE_CURVE('',#7722,#7731,#4290,.T.);
#9767=EDGE_CURVE('',#7732,#7721,#4291,.T.);
#9768=EDGE_CURVE('',#7729,#7732,#4292,.T.);
#9769=EDGE_CURVE('',#7731,#7715,#4293,.T.);
#9770=EDGE_CURVE('',#7730,#7713,#4294,.T.);
#9771=EDGE_CURVE('',#7647,#7636,#4295,.T.);
#9772=EDGE_CURVE('',#7645,#7634,#4296,.T.);
#9773=EDGE_CURVE('',#7641,#7646,#4297,.T.);
#9774=EDGE_CURVE('',#7643,#7648,#4298,.T.);
#9775=EDGE_CURVE('',#7637,#7642,#4299,.T.);
#9776=EDGE_CURVE('',#7639,#7644,#4300,.T.);
#9777=EDGE_CURVE('',#7633,#7638,#4301,.T.);
#9778=EDGE_CURVE('',#7635,#7640,#4302,.T.);
#9779=EDGE_CURVE('',#7693,#7733,#4303,.T.);
#9780=EDGE_CURVE('',#7733,#7733,#1314,.T.);
#9781=EDGE_CURVE('',#7734,#7734,#1315,.T.);
#9782=EDGE_CURVE('',#7734,#7735,#4304,.T.);
#9783=EDGE_CURVE('',#7735,#7735,#1316,.T.);
#9784=EDGE_CURVE('',#7687,#7736,#4305,.T.);
#9785=EDGE_CURVE('',#7736,#7736,#1317,.T.);
#9786=EDGE_CURVE('',#7675,#7737,#4306,.T.);
#9787=EDGE_CURVE('',#7737,#7737,#1318,.T.);
#9788=EDGE_CURVE('',#7690,#7738,#4307,.T.);
#9789=EDGE_CURVE('',#7738,#7738,#1319,.T.);
#9790=EDGE_CURVE('',#7739,#7739,#1320,.T.);
#9791=EDGE_CURVE('',#7739,#7740,#4308,.T.);
#9792=EDGE_CURVE('',#7740,#7740,#1321,.T.);
#9793=EDGE_CURVE('',#7741,#7741,#1322,.T.);
#9794=EDGE_CURVE('',#7741,#7742,#4309,.T.);
#9795=EDGE_CURVE('',#7742,#7742,#1323,.T.);
#9796=EDGE_CURVE('',#7684,#7743,#4310,.T.);
#9797=EDGE_CURVE('',#7743,#7743,#1324,.T.);
#9798=EDGE_CURVE('',#7672,#7744,#4311,.T.);
#9799=EDGE_CURVE('',#7744,#7744,#1325,.T.);
#9800=EDGE_CURVE('',#7681,#7745,#4312,.T.);
#9801=EDGE_CURVE('',#7745,#7745,#1326,.T.);
#9802=EDGE_CURVE('',#7678,#7746,#4313,.T.);
#9803=EDGE_CURVE('',#7746,#7746,#1327,.T.);
#9804=EDGE_CURVE('',#7669,#7747,#4314,.T.);
#9805=EDGE_CURVE('',#7747,#7747,#1328,.T.);
#9806=EDGE_CURVE('',#7666,#7748,#4315,.T.);
#9807=EDGE_CURVE('',#7748,#7748,#1329,.T.);
#9808=EDGE_CURVE('',#7663,#7749,#4316,.T.);
#9809=EDGE_CURVE('',#7749,#7749,#1330,.T.);
#9810=EDGE_CURVE('',#7657,#7750,#4317,.T.);
#9811=EDGE_CURVE('',#7750,#7750,#1331,.T.);
#9812=EDGE_CURVE('',#7660,#7751,#4318,.T.);
#9813=EDGE_CURVE('',#7751,#7751,#1332,.T.);
#9814=EDGE_CURVE('',#7752,#7753,#4319,.T.);
#9815=EDGE_CURVE('',#7754,#7753,#4320,.T.);
#9816=EDGE_CURVE('',#7755,#7754,#4321,.T.);
#9817=EDGE_CURVE('',#7755,#7752,#4322,.T.);
#9818=EDGE_CURVE('',#7756,#7752,#4323,.T.);
#9819=EDGE_CURVE('',#7757,#7755,#4324,.T.);
#9820=EDGE_CURVE('',#7757,#7756,#4325,.T.);
#9821=EDGE_CURVE('',#7650,#7757,#4326,.T.);
#9822=EDGE_CURVE('',#7652,#7756,#4327,.T.);
#9823=EDGE_CURVE('',#7758,#7651,#4328,.T.);
#9824=EDGE_CURVE('',#7759,#7649,#4329,.T.);
#9825=EDGE_CURVE('',#7759,#7758,#4330,.T.);
#9826=EDGE_CURVE('',#7760,#7758,#1333,.T.);
#9827=EDGE_CURVE('',#7761,#7759,#1334,.T.);
#9828=EDGE_CURVE('',#7761,#7760,#4331,.T.);
#9829=EDGE_CURVE('',#7654,#7761,#4332,.T.);
#9830=EDGE_CURVE('',#7656,#7760,#4333,.T.);
#9831=EDGE_CURVE('',#7762,#7655,#4334,.T.);
#9832=EDGE_CURVE('',#7763,#7653,#4335,.T.);
#9833=EDGE_CURVE('',#7763,#7762,#4336,.T.);
#9834=EDGE_CURVE('',#7764,#7762,#1335,.T.);
#9835=EDGE_CURVE('',#7765,#7763,#1336,.T.);
#9836=EDGE_CURVE('',#7765,#7764,#4337,.T.);
#9837=EDGE_CURVE('',#7766,#7764,#4338,.T.);
#9838=EDGE_CURVE('',#7767,#7765,#4339,.T.);
#9839=EDGE_CURVE('',#7767,#7766,#4340,.T.);
#9840=EDGE_CURVE('',#7768,#7766,#1337,.T.);
#9841=EDGE_CURVE('',#7769,#7767,#1338,.T.);
#9842=EDGE_CURVE('',#7769,#7768,#4341,.T.);
#9843=EDGE_CURVE('',#7770,#7768,#4342,.T.);
#9844=EDGE_CURVE('',#7771,#7769,#4343,.T.);
#9845=EDGE_CURVE('',#7771,#7770,#4344,.T.);
#9846=EDGE_CURVE('',#7725,#7697,#4345,.T.);
#9847=EDGE_CURVE('',#7723,#7772,#4346,.T.);
#9848=EDGE_CURVE('',#7702,#7772,#4347,.T.);
#9849=EDGE_CURVE('',#7729,#7770,#4348,.T.);
#9850=EDGE_CURVE('',#7773,#7771,#4349,.T.);
#9851=EDGE_CURVE('',#7773,#7698,#4350,.T.);
#9852=EDGE_CURVE('',#7774,#7699,#4351,.T.);
#9853=EDGE_CURVE('',#7774,#7773,#4352,.T.);
#9854=EDGE_CURVE('',#7775,#7696,#4353,.T.);
#9855=EDGE_CURVE('',#7776,#7774,#4354,.T.);
#9856=EDGE_CURVE('',#7776,#7777,#4355,.T.);
#9857=EDGE_CURVE('',#7732,#7777,#4356,.T.);
#9858=EDGE_CURVE('',#7778,#7719,#4357,.T.);
#9859=EDGE_CURVE('',#7775,#7778,#4358,.T.);
#9860=EDGE_CURVE('',#7779,#7777,#4359,.T.);
#9861=EDGE_CURVE('',#7780,#7776,#4360,.T.);
#9862=EDGE_CURVE('',#7780,#7779,#4361,.T.);
#9863=EDGE_CURVE('',#7781,#7779,#4362,.T.);
#9864=EDGE_CURVE('',#7782,#7780,#4363,.T.);
#9865=EDGE_CURVE('',#7782,#7781,#4364,.T.);
#9866=EDGE_CURVE('',#7720,#7781,#4365,.T.);
#9867=EDGE_CURVE('',#7778,#7782,#4366,.T.);
#9868=EDGE_CURVE('',#7726,#7775,#4367,.T.);
#9869=EDGE_CURVE('',#7753,#7772,#4368,.T.);
#9870=EDGE_CURVE('',#7754,#7724,#4369,.T.);
#9871=EDGE_CURVE('',#7718,#7707,#4370,.T.);
#9872=EDGE_CURVE('',#7717,#7708,#4371,.T.);
#9873=EDGE_CURVE('',#7783,#7784,#1339,.T.);
#9874=EDGE_CURVE('',#7783,#7785,#4372,.T.);
#9875=EDGE_CURVE('',#7785,#7786,#1340,.T.);
#9876=EDGE_CURVE('',#7784,#7786,#4373,.T.);
#9877=EDGE_CURVE('',#7787,#7788,#1341,.T.);
#9878=EDGE_CURVE('',#7789,#7788,#4374,.T.);
#9879=EDGE_CURVE('',#7790,#7789,#1342,.T.);
#9880=EDGE_CURVE('',#7787,#7790,#4375,.T.);
#9881=EDGE_CURVE('',#7789,#7791,#4376,.T.);
#9882=EDGE_CURVE('',#7791,#7783,#4377,.T.);
#9883=EDGE_CURVE('',#7790,#7784,#4378,.T.);
#9884=EDGE_CURVE('',#7792,#7792,#1343,.T.);
#9885=EDGE_CURVE('',#7792,#7793,#1344,.T.);
#9886=EDGE_CURVE('',#7794,#7793,#1345,.T.);
#9887=EDGE_CURVE('',#7793,#7794,#1346,.T.);
#9888=EDGE_CURVE('',#7795,#7795,#1347,.T.);
#9889=EDGE_CURVE('',#7795,#7796,#1348,.T.);
#9890=EDGE_CURVE('',#7797,#7796,#1349,.T.);
#9891=EDGE_CURVE('',#7796,#7797,#1350,.T.);
#9892=EDGE_CURVE('',#7798,#7798,#1351,.T.);
#9893=EDGE_CURVE('',#7798,#7794,#4379,.T.);
#9894=EDGE_CURVE('',#7799,#7799,#1352,.T.);
#9895=EDGE_CURVE('',#7799,#7797,#4380,.T.);
#9896=EDGE_CURVE('',#7786,#7785,#4381,.T.);
#9897=EDGE_CURVE('',#7800,#7801,#4382,.T.);
#9898=EDGE_CURVE('',#7801,#7802,#4383,.T.);
#9899=EDGE_CURVE('',#7802,#7803,#4384,.T.);
#9900=EDGE_CURVE('',#7803,#7800,#4385,.T.);
#9901=EDGE_CURVE('',#7804,#7805,#4386,.T.);
#9902=EDGE_CURVE('',#7803,#7805,#4387,.T.);
#9903=EDGE_CURVE('',#7802,#7804,#4388,.T.);
#9904=EDGE_CURVE('',#7806,#7804,#4389,.T.);
#9905=EDGE_CURVE('',#7801,#7806,#4390,.T.);
#9906=EDGE_CURVE('',#7788,#7806,#4391,.T.);
#9907=EDGE_CURVE('',#7800,#7791,#4392,.T.);
#9908=EDGE_CURVE('',#7805,#7787,#4393,.T.);
#9909=EDGE_CURVE('',#7807,#7808,#4394,.T.);
#9910=EDGE_CURVE('',#7809,#7807,#4395,.T.);
#9911=EDGE_CURVE('',#7809,#7810,#4396,.T.);
#9912=EDGE_CURVE('',#7810,#7808,#4397,.T.);
#9913=EDGE_CURVE('',#7811,#7812,#4398,.T.);
#9914=EDGE_CURVE('',#7813,#7812,#4399,.T.);
#9915=EDGE_CURVE('',#7814,#7813,#4400,.T.);
#9916=EDGE_CURVE('',#7814,#7811,#4401,.T.);
#9917=EDGE_CURVE('',#7815,#7816,#1353,.T.);
#9918=EDGE_CURVE('',#7817,#7815,#4402,.T.);
#9919=EDGE_CURVE('',#7818,#7817,#1354,.T.);
#9920=EDGE_CURVE('',#7816,#7818,#4403,.T.);
#9921=EDGE_CURVE('',#7819,#7820,#1355,.T.);
#9922=EDGE_CURVE('',#7821,#7819,#4404,.T.);
#9923=EDGE_CURVE('',#7822,#7821,#1356,.T.);
#9924=EDGE_CURVE('',#7820,#7822,#4405,.T.);
#9925=EDGE_CURVE('',#7823,#7824,#1357,.T.);
#9926=EDGE_CURVE('',#7825,#7823,#4406,.T.);
#9927=EDGE_CURVE('',#7826,#7825,#1358,.T.);
#9928=EDGE_CURVE('',#7824,#7826,#4407,.T.);
#9929=EDGE_CURVE('',#7827,#7828,#1359,.T.);
#9930=EDGE_CURVE('',#7829,#7827,#4408,.T.);
#9931=EDGE_CURVE('',#7830,#7829,#1360,.T.);
#9932=EDGE_CURVE('',#7828,#7830,#4409,.T.);
#9933=EDGE_CURVE('',#7831,#7820,#4410,.T.);
#9934=EDGE_CURVE('',#7822,#7832,#4411,.T.);
#9935=EDGE_CURVE('',#7832,#7831,#4412,.T.);
#9936=EDGE_CURVE('',#7821,#7818,#4413,.T.);
#9937=EDGE_CURVE('',#7819,#7816,#4414,.T.);
#9938=EDGE_CURVE('',#7833,#7824,#4415,.T.);
#9939=EDGE_CURVE('',#7826,#7834,#4416,.T.);
#9940=EDGE_CURVE('',#7834,#7833,#4417,.T.);
#9941=EDGE_CURVE('',#7823,#7828,#4418,.T.);
#9942=EDGE_CURVE('',#7825,#7830,#4419,.T.);
#9943=EDGE_CURVE('',#7835,#7812,#4420,.T.);
#9944=EDGE_CURVE('',#7829,#7835,#4421,.T.);
#9945=EDGE_CURVE('',#7836,#7827,#4422,.T.);
#9946=EDGE_CURVE('',#7837,#7836,#4423,.T.);
#9947=EDGE_CURVE('',#7838,#7837,#4424,.T.);
#9948=EDGE_CURVE('',#7839,#7838,#4425,.T.);
#9949=EDGE_CURVE('',#7840,#7839,#4426,.T.);
#9950=EDGE_CURVE('',#7841,#7840,#4427,.T.);
#9951=EDGE_CURVE('',#7813,#7841,#4428,.T.);
#9952=EDGE_CURVE('',#7815,#7842,#4429,.T.);
#9953=EDGE_CURVE('',#7842,#7808,#4430,.T.);
#9954=EDGE_CURVE('',#7810,#7843,#4431,.T.);
#9955=EDGE_CURVE('',#7843,#7844,#4432,.T.);
#9956=EDGE_CURVE('',#7844,#7845,#4433,.T.);
#9957=EDGE_CURVE('',#7845,#7846,#4434,.T.);
#9958=EDGE_CURVE('',#7846,#7847,#4435,.T.);
#9959=EDGE_CURVE('',#7847,#7848,#4436,.T.);
#9960=EDGE_CURVE('',#7848,#7817,#4437,.T.);
#9961=EDGE_CURVE('',#7832,#7833,#4438,.T.);
#9962=EDGE_CURVE('',#7848,#7836,#4439,.T.);
#9963=EDGE_CURVE('',#7847,#7837,#4440,.T.);
#9964=EDGE_CURVE('',#7846,#7838,#4441,.T.);
#9965=EDGE_CURVE('',#7845,#7839,#4442,.T.);
#9966=EDGE_CURVE('',#7844,#7840,#4443,.T.);
#9967=EDGE_CURVE('',#7843,#7841,#4444,.T.);
#9968=EDGE_CURVE('',#7809,#7814,#4445,.T.);
#9969=EDGE_CURVE('',#7807,#7811,#4446,.T.);
#9970=EDGE_CURVE('',#7842,#7835,#4447,.T.);
#9971=EDGE_CURVE('',#7831,#7834,#4448,.T.);
#9972=EDGE_CURVE('',#7849,#7850,#4449,.T.);
#9973=EDGE_CURVE('',#7851,#7850,#4450,.T.);
#9974=EDGE_CURVE('',#7851,#7852,#1361,.T.);
#9975=EDGE_CURVE('',#7852,#7849,#286,.F.);
#9976=EDGE_CURVE('',#7853,#7854,#4451,.T.);
#9977=EDGE_CURVE('',#7850,#7854,#287,.T.);
#9978=EDGE_CURVE('',#7849,#7853,#288,.F.);
#9979=EDGE_CURVE('',#7855,#7856,#4452,.T.);
#9980=EDGE_CURVE('',#7854,#7856,#289,.T.);
#9981=EDGE_CURVE('',#7853,#7855,#290,.F.);
#9982=EDGE_CURVE('',#7857,#7858,#4453,.T.);
#9983=EDGE_CURVE('',#7856,#7858,#291,.T.);
#9984=EDGE_CURVE('',#7855,#7857,#292,.F.);
#9985=EDGE_CURVE('',#7859,#7860,#4454,.T.);
#9986=EDGE_CURVE('',#7858,#7860,#293,.T.);
#9987=EDGE_CURVE('',#7857,#7859,#294,.F.);
#9988=EDGE_CURVE('',#7861,#7862,#4455,.T.);
#9989=EDGE_CURVE('',#7860,#7862,#295,.T.);
#9990=EDGE_CURVE('',#7859,#7861,#296,.F.);
#9991=EDGE_CURVE('',#7863,#7864,#4456,.T.);
#9992=EDGE_CURVE('',#7862,#7864,#297,.T.);
#9993=EDGE_CURVE('',#7861,#7863,#298,.F.);
#9994=EDGE_CURVE('',#7865,#7866,#4457,.T.);
#9995=EDGE_CURVE('',#7864,#7866,#299,.T.);
#9996=EDGE_CURVE('',#7863,#7865,#300,.F.);
#9997=EDGE_CURVE('',#7867,#7868,#4458,.T.);
#9998=EDGE_CURVE('',#7866,#7868,#301,.T.);
#9999=EDGE_CURVE('',#7865,#7867,#302,.F.);
#10000=EDGE_CURVE('',#7869,#7870,#4459,.T.);
#10001=EDGE_CURVE('',#7868,#7870,#303,.T.);
#10002=EDGE_CURVE('',#7867,#7869,#304,.F.);
#10003=EDGE_CURVE('',#7871,#7872,#4460,.T.);
#10004=EDGE_CURVE('',#7870,#7872,#305,.T.);
#10005=EDGE_CURVE('',#7869,#7871,#306,.F.);
#10006=EDGE_CURVE('',#7873,#7874,#4461,.T.);
#10007=EDGE_CURVE('',#7872,#7874,#307,.T.);
#10008=EDGE_CURVE('',#7871,#7873,#308,.F.);
#10009=EDGE_CURVE('',#7875,#7876,#4462,.T.);
#10010=EDGE_CURVE('',#7874,#7876,#309,.T.);
#10011=EDGE_CURVE('',#7873,#7875,#310,.F.);
#10012=EDGE_CURVE('',#7877,#7878,#4463,.T.);
#10013=EDGE_CURVE('',#7876,#7878,#311,.T.);
#10014=EDGE_CURVE('',#7875,#7877,#312,.F.);
#10015=EDGE_CURVE('',#7879,#7880,#4464,.T.);
#10016=EDGE_CURVE('',#7878,#7880,#313,.T.);
#10017=EDGE_CURVE('',#7877,#7879,#314,.F.);
#10018=EDGE_CURVE('',#7881,#7882,#4465,.T.);
#10019=EDGE_CURVE('',#7880,#7882,#315,.T.);
#10020=EDGE_CURVE('',#7879,#7881,#316,.F.);
#10021=EDGE_CURVE('',#7883,#7884,#4466,.T.);
#10022=EDGE_CURVE('',#7882,#7884,#317,.T.);
#10023=EDGE_CURVE('',#7881,#7883,#318,.F.);
#10024=EDGE_CURVE('',#7885,#7886,#4467,.T.);
#10025=EDGE_CURVE('',#7884,#7886,#319,.T.);
#10026=EDGE_CURVE('',#7883,#7885,#320,.F.);
#10027=EDGE_CURVE('',#7887,#7888,#4468,.T.);
#10028=EDGE_CURVE('',#7887,#7889,#321,.F.);
#10029=EDGE_CURVE('',#7889,#7890,#1362,.T.);
#10030=EDGE_CURVE('',#7888,#7890,#322,.T.);
#10031=EDGE_CURVE('',#7891,#7892,#4469,.T.);
#10032=EDGE_CURVE('',#7891,#7889,#1363,.T.);
#10033=EDGE_CURVE('',#7889,#7893,#429,.T.);
#10034=EDGE_CURVE('',#7894,#7893,#4470,.T.);
#10035=EDGE_CURVE('',#7892,#7894,#59,.T.);
#10036=EDGE_CURVE('',#7895,#7896,#4471,.T.);
#10037=EDGE_CURVE('',#7896,#7897,#60,.T.);
#10038=EDGE_CURVE('',#7898,#7897,#4472,.T.);
#10039=EDGE_CURVE('',#7895,#7898,#61,.T.);
#10040=EDGE_CURVE('',#7899,#7900,#4473,.T.);
#10041=EDGE_CURVE('',#7900,#7896,#62,.T.);
#10042=EDGE_CURVE('',#7899,#7895,#63,.T.);
#10043=EDGE_CURVE('',#7901,#7902,#4474,.T.);
#10044=EDGE_CURVE('',#7902,#7900,#64,.T.);
#10045=EDGE_CURVE('',#7901,#7899,#65,.T.);
#10046=EDGE_CURVE('',#7903,#7904,#4475,.T.);
#10047=EDGE_CURVE('',#7904,#7902,#66,.T.);
#10048=EDGE_CURVE('',#7903,#7901,#67,.T.);
#10049=EDGE_CURVE('',#7905,#7906,#4476,.T.);
#10050=EDGE_CURVE('',#7906,#7904,#68,.T.);
#10051=EDGE_CURVE('',#7905,#7903,#69,.T.);
#10052=EDGE_CURVE('',#7907,#7908,#4477,.T.);
#10053=EDGE_CURVE('',#7908,#7906,#70,.T.);
#10054=EDGE_CURVE('',#7907,#7905,#71,.T.);
#10055=EDGE_CURVE('',#7909,#7910,#4478,.T.);
#10056=EDGE_CURVE('',#7910,#7908,#72,.T.);
#10057=EDGE_CURVE('',#7909,#7907,#73,.T.);
#10058=EDGE_CURVE('',#7911,#7912,#4479,.T.);
#10059=EDGE_CURVE('',#7912,#7910,#74,.T.);
#10060=EDGE_CURVE('',#7911,#7909,#75,.T.);
#10061=EDGE_CURVE('',#7913,#7914,#4480,.T.);
#10062=EDGE_CURVE('',#7914,#7912,#76,.T.);
#10063=EDGE_CURVE('',#7913,#7911,#77,.T.);
#10064=EDGE_CURVE('',#7915,#7916,#4481,.T.);
#10065=EDGE_CURVE('',#7916,#7914,#78,.T.);
#10066=EDGE_CURVE('',#7915,#7913,#79,.T.);
#10067=EDGE_CURVE('',#7917,#7918,#4482,.T.);
#10068=EDGE_CURVE('',#7918,#7916,#80,.T.);
#10069=EDGE_CURVE('',#7917,#7915,#81,.T.);
#10070=EDGE_CURVE('',#7919,#7920,#4483,.T.);
#10071=EDGE_CURVE('',#7920,#7918,#82,.T.);
#10072=EDGE_CURVE('',#7919,#7917,#83,.T.);
#10073=EDGE_CURVE('',#7921,#7922,#4484,.T.);
#10074=EDGE_CURVE('',#7922,#7920,#84,.T.);
#10075=EDGE_CURVE('',#7921,#7919,#85,.T.);
#10076=EDGE_CURVE('',#7923,#7924,#4485,.T.);
#10077=EDGE_CURVE('',#7924,#7922,#86,.T.);
#10078=EDGE_CURVE('',#7923,#7921,#87,.T.);
#10079=EDGE_CURVE('',#7925,#7926,#4486,.T.);
#10080=EDGE_CURVE('',#7926,#7924,#88,.T.);
#10081=EDGE_CURVE('',#7925,#7923,#89,.T.);
#10082=EDGE_CURVE('',#7927,#7928,#4487,.T.);
#10083=EDGE_CURVE('',#7928,#7926,#90,.T.);
#10084=EDGE_CURVE('',#7927,#7925,#91,.T.);
#10085=EDGE_CURVE('',#7929,#7930,#4488,.T.);
#10086=EDGE_CURVE('',#7930,#7928,#92,.T.);
#10087=EDGE_CURVE('',#7929,#7927,#93,.T.);
#10088=EDGE_CURVE('',#7931,#7932,#4489,.T.);
#10089=EDGE_CURVE('',#7932,#7930,#94,.T.);
#10090=EDGE_CURVE('',#7931,#7929,#95,.T.);
#10091=EDGE_CURVE('',#7933,#7934,#4490,.T.);
#10092=EDGE_CURVE('',#7934,#7932,#96,.T.);
#10093=EDGE_CURVE('',#7933,#7931,#97,.T.);
#10094=EDGE_CURVE('',#7935,#7936,#4491,.T.);
#10095=EDGE_CURVE('',#7937,#7935,#98,.T.);
#10096=EDGE_CURVE('',#7938,#7937,#4492,.T.);
#10097=EDGE_CURVE('',#7938,#7936,#99,.T.);
#10098=EDGE_CURVE('',#7939,#7940,#4493,.T.);
#10099=EDGE_CURVE('',#7941,#7939,#323,.T.);
#10100=EDGE_CURVE('',#7941,#7942,#1364,.T.);
#10101=EDGE_CURVE('',#7942,#7940,#324,.F.);
#10102=EDGE_CURVE('',#7943,#7944,#4494,.T.);
#10103=EDGE_CURVE('',#7939,#7943,#325,.T.);
#10104=EDGE_CURVE('',#7940,#7944,#326,.F.);
#10105=EDGE_CURVE('',#7945,#7946,#4495,.T.);
#10106=EDGE_CURVE('',#7943,#7945,#327,.T.);
#10107=EDGE_CURVE('',#7944,#7946,#328,.F.);
#10108=EDGE_CURVE('',#7947,#7948,#4496,.T.);
#10109=EDGE_CURVE('',#7947,#7949,#100,.T.);
#10110=EDGE_CURVE('',#7949,#7950,#4497,.T.);
#10111=EDGE_CURVE('',#7948,#7950,#101,.T.);
#10112=EDGE_CURVE('',#7951,#7952,#4498,.T.);
#10113=EDGE_CURVE('',#7951,#7947,#102,.T.);
#10114=EDGE_CURVE('',#7952,#7948,#103,.T.);
#10115=EDGE_CURVE('',#7953,#7954,#4499,.T.);
#10116=EDGE_CURVE('',#7953,#7951,#104,.T.);
#10117=EDGE_CURVE('',#7954,#7952,#105,.T.);
#10118=EDGE_CURVE('',#7955,#7956,#4500,.T.);
#10119=EDGE_CURVE('',#7955,#7953,#106,.T.);
#10120=EDGE_CURVE('',#7956,#7954,#107,.T.);
#10121=EDGE_CURVE('',#7957,#7958,#4501,.T.);
#10122=EDGE_CURVE('',#7957,#7955,#108,.T.);
#10123=EDGE_CURVE('',#7958,#7956,#109,.T.);
#10124=EDGE_CURVE('',#7959,#7960,#4502,.T.);
#10125=EDGE_CURVE('',#7959,#7957,#110,.T.);
#10126=EDGE_CURVE('',#7960,#7958,#111,.T.);
#10127=EDGE_CURVE('',#7961,#7962,#4503,.T.);
#10128=EDGE_CURVE('',#7961,#7959,#112,.T.);
#10129=EDGE_CURVE('',#7962,#7960,#113,.T.);
#10130=EDGE_CURVE('',#7963,#7964,#4504,.T.);
#10131=EDGE_CURVE('',#7963,#7961,#114,.T.);
#10132=EDGE_CURVE('',#7964,#7962,#115,.T.);
#10133=EDGE_CURVE('',#7965,#7966,#4505,.T.);
#10134=EDGE_CURVE('',#7966,#7967,#329,.T.);
#10135=EDGE_CURVE('',#7967,#7968,#1365,.T.);
#10136=EDGE_CURVE('',#7968,#7965,#330,.T.);
#10137=EDGE_CURVE('',#7969,#7970,#4506,.T.);
#10138=EDGE_CURVE('',#7970,#7966,#331,.T.);
#10139=EDGE_CURVE('',#7965,#7969,#332,.T.);
#10140=EDGE_CURVE('',#7971,#7972,#4507,.T.);
#10141=EDGE_CURVE('',#7972,#7970,#333,.T.);
#10142=EDGE_CURVE('',#7969,#7971,#334,.T.);
#10143=EDGE_CURVE('',#7973,#7974,#4508,.T.);
#10144=EDGE_CURVE('',#7973,#7975,#335,.T.);
#10145=EDGE_CURVE('',#7976,#7975,#4509,.T.);
#10146=EDGE_CURVE('',#7976,#7974,#336,.T.);
#10147=EDGE_CURVE('',#7974,#7972,#337,.T.);
#10148=EDGE_CURVE('',#7971,#7973,#338,.T.);
#10149=EDGE_CURVE('',#7977,#7978,#1366,.T.);
#10150=EDGE_CURVE('',#7979,#7978,#4510,.T.);
#10151=EDGE_CURVE('',#7980,#7979,#4511,.T.);
#10152=EDGE_CURVE('',#7977,#7980,#4512,.T.);
#10153=EDGE_CURVE('',#7981,#7982,#116,.T.);
#10154=EDGE_CURVE('',#7982,#7980,#4513,.T.);
#10155=EDGE_CURVE('',#7981,#7979,#4514,.T.);
#10156=EDGE_CURVE('',#7983,#7981,#117,.T.);
#10157=EDGE_CURVE('',#7978,#7984,#4515,.T.);
#10158=EDGE_CURVE('',#7984,#7983,#4516,.T.);
#10159=EDGE_CURVE('',#7982,#7985,#118,.T.);
#10160=EDGE_CURVE('',#7985,#7986,#4517,.T.);
#10161=EDGE_CURVE('',#7986,#7977,#4518,.T.);
#10162=EDGE_CURVE('',#7987,#7988,#4519,.T.);
#10163=EDGE_CURVE('',#7989,#7987,#4520,.T.);
#10164=EDGE_CURVE('',#7990,#7989,#4521,.T.);
#10165=EDGE_CURVE('',#7988,#7990,#1367,.T.);
#10166=EDGE_CURVE('',#7991,#7992,#119,.T.);
#10167=EDGE_CURVE('',#7992,#7993,#4522,.T.);
#10168=EDGE_CURVE('',#7993,#7990,#4523,.T.);
#10169=EDGE_CURVE('',#7991,#7989,#4524,.T.);
#10170=EDGE_CURVE('',#7994,#7991,#120,.T.);
#10171=EDGE_CURVE('',#7994,#7987,#4525,.T.);
#10172=EDGE_CURVE('',#7995,#7994,#121,.T.);
#10173=EDGE_CURVE('',#7988,#7996,#4526,.T.);
#10174=EDGE_CURVE('',#7996,#7995,#4527,.T.);
#10175=EDGE_CURVE('',#7997,#7998,#4528,.T.);
#10176=EDGE_CURVE('',#7999,#7997,#4529,.T.);
#10177=EDGE_CURVE('',#8000,#7999,#4530,.T.);
#10178=EDGE_CURVE('',#7998,#8000,#1368,.T.);
#10179=EDGE_CURVE('',#8001,#8002,#122,.T.);
#10180=EDGE_CURVE('',#8002,#8003,#4531,.T.);
#10181=EDGE_CURVE('',#8003,#8000,#4532,.T.);
#10182=EDGE_CURVE('',#8001,#7999,#4533,.T.);
#10183=EDGE_CURVE('',#8004,#8001,#123,.T.);
#10184=EDGE_CURVE('',#8004,#7997,#4534,.T.);
#10185=EDGE_CURVE('',#8005,#8004,#124,.T.);
#10186=EDGE_CURVE('',#7998,#8006,#4535,.T.);
#10187=EDGE_CURVE('',#8006,#8005,#4536,.T.);
#10188=EDGE_CURVE('',#8007,#8008,#4537,.T.);
#10189=EDGE_CURVE('',#8009,#8007,#4538,.T.);
#10190=EDGE_CURVE('',#8010,#8009,#4539,.T.);
#10191=EDGE_CURVE('',#8011,#8010,#1369,.T.);
#10192=EDGE_CURVE('',#8008,#8011,#1370,.T.);
#10193=EDGE_CURVE('',#8012,#8013,#125,.T.);
#10194=EDGE_CURVE('',#8013,#8014,#4540,.T.);
#10195=EDGE_CURVE('',#8014,#8010,#4541,.T.);
#10196=EDGE_CURVE('',#8012,#8009,#4542,.T.);
#10197=EDGE_CURVE('',#8015,#8016,#126,.T.);
#10198=EDGE_CURVE('',#8016,#8012,#127,.T.);
#10199=EDGE_CURVE('',#8015,#8007,#4543,.T.);
#10200=EDGE_CURVE('',#8017,#8015,#128,.T.);
#10201=EDGE_CURVE('',#8008,#8018,#4544,.T.);
#10202=EDGE_CURVE('',#8018,#8017,#4545,.T.);
#10203=EDGE_CURVE('',#7993,#7984,#1371,.T.);
#10204=EDGE_CURVE('',#7992,#7983,#1372,.T.);
#10205=EDGE_CURVE('',#7990,#7978,#1373,.T.);
#10206=EDGE_CURVE('',#8019,#8019,#1374,.T.);
#10207=EDGE_CURVE('',#8019,#8011,#4546,.T.);
#10208=EDGE_CURVE('',#8010,#7998,#1375,.T.);
#10209=EDGE_CURVE('',#8000,#7988,#1376,.T.);
#10210=EDGE_CURVE('',#7977,#8008,#1377,.T.);
#10211=EDGE_CURVE('',#7942,#7967,#339,.T.);
#10212=EDGE_CURVE('',#7968,#7941,#340,.T.);
#10213=EDGE_CURVE('',#8020,#8020,#1378,.T.);
#10214=EDGE_CURVE('',#8020,#8021,#4547,.T.);
#10215=EDGE_CURVE('',#8021,#8021,#1379,.T.);
#10216=EDGE_CURVE('',#8022,#8022,#1380,.T.);
#10217=EDGE_CURVE('',#8022,#8020,#1381,.T.);
#10218=EDGE_CURVE('',#8002,#7995,#1382,.T.);
#10219=EDGE_CURVE('',#8013,#8005,#1383,.T.);
#10220=EDGE_CURVE('',#8016,#8022,#4548,.T.);
#10221=EDGE_CURVE('',#7985,#8017,#1384,.T.);
#10222=EDGE_CURVE('',#8014,#8006,#1385,.T.);
#10223=EDGE_CURVE('',#8003,#7996,#1386,.T.);
#10224=EDGE_CURVE('',#7986,#8018,#1387,.T.);
#10225=EDGE_CURVE('',#7976,#8023,#4549,.T.);
#10226=EDGE_CURVE('',#8023,#7964,#129,.T.);
#10227=EDGE_CURVE('',#7950,#8024,#4550,.T.);
#10228=EDGE_CURVE('',#8025,#8024,#130,.T.);
#10229=EDGE_CURVE('',#7946,#8025,#341,.F.);
#10230=EDGE_CURVE('',#7945,#8026,#342,.T.);
#10231=EDGE_CURVE('',#8026,#7949,#4551,.T.);
#10232=EDGE_CURVE('',#8027,#7963,#131,.T.);
#10233=EDGE_CURVE('',#8027,#7975,#4552,.T.);
#10234=EDGE_CURVE('',#8023,#8027,#4553,.T.);
#10235=EDGE_CURVE('',#8028,#8028,#1388,.T.);
#10236=EDGE_CURVE('',#8029,#8029,#1389,.T.);
#10237=EDGE_CURVE('',#8029,#8030,#4554,.T.);
#10238=EDGE_CURVE('',#8030,#8030,#1390,.T.);
#10239=EDGE_CURVE('',#8024,#8026,#4555,.T.);
#10240=EDGE_CURVE('',#8026,#8025,#1391,.T.);
#10241=EDGE_CURVE('',#8030,#8028,#1392,.T.);
#10242=EDGE_CURVE('',#8031,#8031,#1393,.T.);
#10243=EDGE_CURVE('',#8031,#8032,#1394,.T.);
#10244=EDGE_CURVE('',#8033,#8032,#1395,.T.);
#10245=EDGE_CURVE('',#8032,#8033,#1396,.T.);
#10246=EDGE_CURVE('',#8034,#8034,#1397,.T.);
#10247=EDGE_CURVE('',#8034,#8035,#4556,.T.);
#10248=EDGE_CURVE('',#8035,#8035,#1398,.T.);
#10249=EDGE_CURVE('',#8036,#8036,#1399,.T.);
#10250=EDGE_CURVE('',#8036,#8037,#4557,.T.);
#10251=EDGE_CURVE('',#8037,#8037,#1400,.T.);
#10252=EDGE_CURVE('',#8038,#8038,#1401,.T.);
#10253=EDGE_CURVE('',#8039,#8040,#1402,.T.);
#10254=EDGE_CURVE('',#8040,#8041,#1403,.T.);
#10255=EDGE_CURVE('',#8041,#8042,#1404,.T.);
#10256=EDGE_CURVE('',#8042,#8043,#1405,.T.);
#10257=EDGE_CURVE('',#8043,#8044,#1406,.T.);
#10258=EDGE_CURVE('',#8044,#8033,#4558,.T.);
#10259=EDGE_CURVE('',#8044,#8045,#1407,.T.);
#10260=EDGE_CURVE('',#8045,#8046,#1408,.T.);
#10261=EDGE_CURVE('',#8046,#8047,#1409,.T.);
#10262=EDGE_CURVE('',#8047,#8039,#1410,.T.);
#10263=EDGE_CURVE('',#8025,#8026,#1411,.T.);
#10264=EDGE_CURVE('',#8043,#8048,#1412,.T.);
#10265=EDGE_CURVE('',#8048,#8045,#1413,.T.);
#10266=EDGE_CURVE('',#8041,#8042,#1414,.T.);
#10267=EDGE_CURVE('',#8039,#8040,#1415,.T.);
#10268=EDGE_CURVE('',#8046,#8047,#1416,.T.);
#10269=EDGE_CURVE('',#8049,#8049,#1417,.T.);
#10270=EDGE_CURVE('',#8049,#8048,#4559,.T.);
#10271=EDGE_CURVE('',#8045,#8043,#1418,.T.);
#10272=EDGE_CURVE('',#8050,#8050,#1419,.T.);
#10273=EDGE_CURVE('',#8050,#8051,#4560,.T.);
#10274=EDGE_CURVE('',#8042,#8051,#1420,.T.);
#10275=EDGE_CURVE('',#8051,#8041,#1421,.T.);
#10276=EDGE_CURVE('',#8052,#8052,#1422,.T.);
#10277=EDGE_CURVE('',#8052,#8053,#4561,.T.);
#10278=EDGE_CURVE('',#8040,#8053,#1423,.T.);
#10279=EDGE_CURVE('',#8053,#8039,#1424,.T.);
#10280=EDGE_CURVE('',#8054,#8054,#1425,.T.);
#10281=EDGE_CURVE('',#8054,#8055,#4562,.T.);
#10282=EDGE_CURVE('',#8047,#8055,#1426,.T.);
#10283=EDGE_CURVE('',#8055,#8046,#1427,.T.);
#10284=EDGE_CURVE('',#8038,#8056,#4563,.T.);
#10285=EDGE_CURVE('',#8056,#8056,#1428,.T.);
#10286=EDGE_CURVE('',#8057,#8058,#4564,.T.);
#10287=EDGE_CURVE('',#8059,#8058,#4565,.T.);
#10288=EDGE_CURVE('',#8060,#8059,#4566,.T.);
#10289=EDGE_CURVE('',#8060,#8057,#4567,.T.);
#10290=EDGE_CURVE('',#8061,#8057,#4568,.T.);
#10291=EDGE_CURVE('',#8062,#8060,#4569,.T.);
#10292=EDGE_CURVE('',#8062,#8061,#4570,.T.);
#10293=EDGE_CURVE('',#8063,#8061,#4571,.T.);
#10294=EDGE_CURVE('',#8064,#8062,#4572,.T.);
#10295=EDGE_CURVE('',#8064,#8063,#4573,.T.);
#10296=EDGE_CURVE('',#8065,#8063,#4574,.T.);
#10297=EDGE_CURVE('',#8066,#8064,#4575,.T.);
#10298=EDGE_CURVE('',#8066,#8065,#4576,.T.);
#10299=EDGE_CURVE('',#8067,#8065,#4577,.T.);
#10300=EDGE_CURVE('',#8068,#8066,#4578,.T.);
#10301=EDGE_CURVE('',#8068,#8067,#4579,.T.);
#10302=EDGE_CURVE('',#8069,#8067,#4580,.T.);
#10303=EDGE_CURVE('',#8070,#8068,#4581,.T.);
#10304=EDGE_CURVE('',#8070,#8069,#4582,.T.);
#10305=EDGE_CURVE('',#8071,#8069,#4583,.T.);
#10306=EDGE_CURVE('',#8072,#8070,#4584,.T.);
#10307=EDGE_CURVE('',#8072,#8071,#4585,.T.);
#10308=EDGE_CURVE('',#8073,#8071,#4586,.T.);
#10309=EDGE_CURVE('',#8074,#8072,#4587,.T.);
#10310=EDGE_CURVE('',#8074,#8073,#4588,.T.);
#10311=EDGE_CURVE('',#8075,#8073,#4589,.T.);
#10312=EDGE_CURVE('',#8076,#8074,#4590,.T.);
#10313=EDGE_CURVE('',#8076,#8075,#4591,.T.);
#10314=EDGE_CURVE('',#8077,#8075,#4592,.T.);
#10315=EDGE_CURVE('',#8078,#8076,#4593,.T.);
#10316=EDGE_CURVE('',#8078,#8077,#4594,.T.);
#10317=EDGE_CURVE('',#8079,#8077,#4595,.T.);
#10318=EDGE_CURVE('',#8080,#8078,#4596,.T.);
#10319=EDGE_CURVE('',#8080,#8079,#4597,.T.);
#10320=EDGE_CURVE('',#8081,#8079,#4598,.T.);
#10321=EDGE_CURVE('',#8082,#8080,#4599,.T.);
#10322=EDGE_CURVE('',#8082,#8081,#4600,.T.);
#10323=EDGE_CURVE('',#8083,#8081,#4601,.T.);
#10324=EDGE_CURVE('',#8084,#8082,#4602,.T.);
#10325=EDGE_CURVE('',#8084,#8083,#4603,.T.);
#10326=EDGE_CURVE('',#8085,#8083,#4604,.T.);
#10327=EDGE_CURVE('',#8086,#8084,#4605,.T.);
#10328=EDGE_CURVE('',#8086,#8085,#4606,.T.);
#10329=EDGE_CURVE('',#8087,#8085,#4607,.T.);
#10330=EDGE_CURVE('',#8088,#8086,#4608,.T.);
#10331=EDGE_CURVE('',#8088,#8087,#4609,.T.);
#10332=EDGE_CURVE('',#8089,#8087,#4610,.T.);
#10333=EDGE_CURVE('',#8090,#8088,#4611,.T.);
#10334=EDGE_CURVE('',#8090,#8089,#4612,.T.);
#10335=EDGE_CURVE('',#8091,#8089,#4613,.T.);
#10336=EDGE_CURVE('',#8092,#8090,#4614,.T.);
#10337=EDGE_CURVE('',#8092,#8091,#4615,.T.);
#10338=EDGE_CURVE('',#8093,#8091,#4616,.T.);
#10339=EDGE_CURVE('',#8094,#8092,#4617,.T.);
#10340=EDGE_CURVE('',#8094,#8093,#4618,.T.);
#10341=EDGE_CURVE('',#8095,#8093,#4619,.T.);
#10342=EDGE_CURVE('',#8096,#8094,#4620,.T.);
#10343=EDGE_CURVE('',#8096,#8095,#4621,.T.);
#10344=EDGE_CURVE('',#8097,#8095,#4622,.T.);
#10345=EDGE_CURVE('',#8098,#8096,#4623,.T.);
#10346=EDGE_CURVE('',#8098,#8097,#4624,.T.);
#10347=EDGE_CURVE('',#8099,#8097,#4625,.T.);
#10348=EDGE_CURVE('',#8100,#8098,#4626,.T.);
#10349=EDGE_CURVE('',#8100,#8099,#4627,.T.);
#10350=EDGE_CURVE('',#8101,#8099,#4628,.T.);
#10351=EDGE_CURVE('',#8102,#8100,#4629,.T.);
#10352=EDGE_CURVE('',#8102,#8101,#4630,.T.);
#10353=EDGE_CURVE('',#8103,#8101,#4631,.T.);
#10354=EDGE_CURVE('',#8104,#8102,#4632,.T.);
#10355=EDGE_CURVE('',#8104,#8103,#4633,.T.);
#10356=EDGE_CURVE('',#8105,#8103,#4634,.T.);
#10357=EDGE_CURVE('',#8106,#8104,#4635,.T.);
#10358=EDGE_CURVE('',#8106,#8105,#4636,.T.);
#10359=EDGE_CURVE('',#8107,#8105,#4637,.T.);
#10360=EDGE_CURVE('',#8108,#8106,#4638,.T.);
#10361=EDGE_CURVE('',#8108,#8107,#4639,.T.);
#10362=EDGE_CURVE('',#8109,#8107,#4640,.T.);
#10363=EDGE_CURVE('',#8110,#8108,#4641,.T.);
#10364=EDGE_CURVE('',#8110,#8109,#4642,.T.);
#10365=EDGE_CURVE('',#8111,#8109,#4643,.T.);
#10366=EDGE_CURVE('',#8112,#8110,#4644,.T.);
#10367=EDGE_CURVE('',#8112,#8111,#4645,.T.);
#10368=EDGE_CURVE('',#8113,#8111,#4646,.T.);
#10369=EDGE_CURVE('',#8114,#8112,#4647,.T.);
#10370=EDGE_CURVE('',#8114,#8113,#4648,.T.);
#10371=EDGE_CURVE('',#8115,#8113,#4649,.T.);
#10372=EDGE_CURVE('',#8116,#8114,#4650,.T.);
#10373=EDGE_CURVE('',#8116,#8115,#4651,.T.);
#10374=EDGE_CURVE('',#8117,#8115,#4652,.T.);
#10375=EDGE_CURVE('',#8118,#8116,#4653,.T.);
#10376=EDGE_CURVE('',#8118,#8117,#4654,.T.);
#10377=EDGE_CURVE('',#8119,#8117,#4655,.T.);
#10378=EDGE_CURVE('',#8120,#8118,#4656,.T.);
#10379=EDGE_CURVE('',#8120,#8119,#4657,.T.);
#10380=EDGE_CURVE('',#8121,#8119,#4658,.T.);
#10381=EDGE_CURVE('',#8122,#8120,#4659,.T.);
#10382=EDGE_CURVE('',#8122,#8121,#4660,.T.);
#10383=EDGE_CURVE('',#8123,#8121,#4661,.T.);
#10384=EDGE_CURVE('',#8124,#8122,#4662,.T.);
#10385=EDGE_CURVE('',#8124,#8123,#4663,.T.);
#10386=EDGE_CURVE('',#8125,#8123,#4664,.T.);
#10387=EDGE_CURVE('',#8126,#8124,#4665,.T.);
#10388=EDGE_CURVE('',#8126,#8125,#4666,.T.);
#10389=EDGE_CURVE('',#8127,#8125,#4667,.T.);
#10390=EDGE_CURVE('',#8128,#8126,#4668,.T.);
#10391=EDGE_CURVE('',#8128,#8127,#4669,.T.);
#10392=EDGE_CURVE('',#8129,#8127,#4670,.T.);
#10393=EDGE_CURVE('',#8130,#8128,#4671,.T.);
#10394=EDGE_CURVE('',#8130,#8129,#4672,.T.);
#10395=EDGE_CURVE('',#8131,#8129,#4673,.T.);
#10396=EDGE_CURVE('',#8132,#8130,#4674,.T.);
#10397=EDGE_CURVE('',#8132,#8131,#4675,.T.);
#10398=EDGE_CURVE('',#8133,#8131,#4676,.T.);
#10399=EDGE_CURVE('',#8134,#8132,#4677,.T.);
#10400=EDGE_CURVE('',#8134,#8133,#4678,.T.);
#10401=EDGE_CURVE('',#8135,#8133,#4679,.T.);
#10402=EDGE_CURVE('',#8136,#8134,#4680,.T.);
#10403=EDGE_CURVE('',#8136,#8135,#4681,.T.);
#10404=EDGE_CURVE('',#8137,#8135,#4682,.T.);
#10405=EDGE_CURVE('',#8138,#8136,#4683,.T.);
#10406=EDGE_CURVE('',#8138,#8137,#4684,.T.);
#10407=EDGE_CURVE('',#8139,#8137,#4685,.T.);
#10408=EDGE_CURVE('',#8140,#8138,#4686,.T.);
#10409=EDGE_CURVE('',#8140,#8139,#4687,.T.);
#10410=EDGE_CURVE('',#8141,#8139,#4688,.T.);
#10411=EDGE_CURVE('',#8142,#8140,#4689,.T.);
#10412=EDGE_CURVE('',#8142,#8141,#4690,.T.);
#10413=EDGE_CURVE('',#8143,#8141,#4691,.T.);
#10414=EDGE_CURVE('',#8144,#8142,#4692,.T.);
#10415=EDGE_CURVE('',#8144,#8143,#4693,.T.);
#10416=EDGE_CURVE('',#8145,#8143,#4694,.T.);
#10417=EDGE_CURVE('',#8146,#8144,#4695,.T.);
#10418=EDGE_CURVE('',#8146,#8145,#4696,.T.);
#10419=EDGE_CURVE('',#8147,#8145,#4697,.T.);
#10420=EDGE_CURVE('',#8148,#8146,#4698,.T.);
#10421=EDGE_CURVE('',#8148,#8147,#4699,.T.);
#10422=EDGE_CURVE('',#8149,#8147,#4700,.T.);
#10423=EDGE_CURVE('',#8150,#8148,#4701,.T.);
#10424=EDGE_CURVE('',#8150,#8149,#4702,.T.);
#10425=EDGE_CURVE('',#8151,#8149,#4703,.T.);
#10426=EDGE_CURVE('',#8152,#8150,#4704,.T.);
#10427=EDGE_CURVE('',#8152,#8151,#4705,.T.);
#10428=EDGE_CURVE('',#8153,#8151,#4706,.T.);
#10429=EDGE_CURVE('',#8154,#8152,#4707,.T.);
#10430=EDGE_CURVE('',#8154,#8153,#4708,.T.);
#10431=EDGE_CURVE('',#8155,#8153,#4709,.T.);
#10432=EDGE_CURVE('',#8156,#8154,#4710,.T.);
#10433=EDGE_CURVE('',#8156,#8155,#4711,.T.);
#10434=EDGE_CURVE('',#8157,#8155,#4712,.T.);
#10435=EDGE_CURVE('',#8158,#8156,#4713,.T.);
#10436=EDGE_CURVE('',#8158,#8157,#4714,.T.);
#10437=EDGE_CURVE('',#8159,#8157,#4715,.T.);
#10438=EDGE_CURVE('',#8160,#8158,#4716,.T.);
#10439=EDGE_CURVE('',#8160,#8159,#4717,.T.);
#10440=EDGE_CURVE('',#8161,#8159,#4718,.T.);
#10441=EDGE_CURVE('',#8162,#8160,#4719,.T.);
#10442=EDGE_CURVE('',#8162,#8161,#4720,.T.);
#10443=EDGE_CURVE('',#8163,#8161,#4721,.T.);
#10444=EDGE_CURVE('',#8164,#8162,#4722,.T.);
#10445=EDGE_CURVE('',#8164,#8163,#4723,.T.);
#10446=EDGE_CURVE('',#8165,#8163,#4724,.T.);
#10447=EDGE_CURVE('',#8166,#8164,#4725,.T.);
#10448=EDGE_CURVE('',#8166,#8165,#4726,.T.);
#10449=EDGE_CURVE('',#8167,#8165,#4727,.T.);
#10450=EDGE_CURVE('',#8168,#8166,#4728,.T.);
#10451=EDGE_CURVE('',#8168,#8167,#4729,.T.);
#10452=EDGE_CURVE('',#8169,#8167,#4730,.T.);
#10453=EDGE_CURVE('',#8170,#8168,#4731,.T.);
#10454=EDGE_CURVE('',#8170,#8169,#4732,.T.);
#10455=EDGE_CURVE('',#8171,#8169,#4733,.T.);
#10456=EDGE_CURVE('',#8172,#8170,#4734,.T.);
#10457=EDGE_CURVE('',#8172,#8171,#4735,.T.);
#10458=EDGE_CURVE('',#8173,#8171,#4736,.T.);
#10459=EDGE_CURVE('',#8174,#8172,#4737,.T.);
#10460=EDGE_CURVE('',#8174,#8173,#4738,.T.);
#10461=EDGE_CURVE('',#8175,#8173,#4739,.T.);
#10462=EDGE_CURVE('',#8176,#8174,#4740,.T.);
#10463=EDGE_CURVE('',#8176,#8175,#4741,.T.);
#10464=EDGE_CURVE('',#8177,#8175,#4742,.T.);
#10465=EDGE_CURVE('',#8178,#8176,#4743,.T.);
#10466=EDGE_CURVE('',#8178,#8177,#4744,.T.);
#10467=EDGE_CURVE('',#8179,#8177,#4745,.T.);
#10468=EDGE_CURVE('',#8180,#8178,#4746,.T.);
#10469=EDGE_CURVE('',#8180,#8179,#4747,.T.);
#10470=EDGE_CURVE('',#8181,#8179,#4748,.T.);
#10471=EDGE_CURVE('',#8182,#8180,#4749,.T.);
#10472=EDGE_CURVE('',#8182,#8181,#4750,.T.);
#10473=EDGE_CURVE('',#8183,#8181,#4751,.T.);
#10474=EDGE_CURVE('',#8184,#8182,#4752,.T.);
#10475=EDGE_CURVE('',#8184,#8183,#4753,.T.);
#10476=EDGE_CURVE('',#8185,#8183,#4754,.T.);
#10477=EDGE_CURVE('',#8186,#8184,#4755,.T.);
#10478=EDGE_CURVE('',#8186,#8185,#4756,.T.);
#10479=EDGE_CURVE('',#8187,#8185,#4757,.T.);
#10480=EDGE_CURVE('',#8188,#8186,#4758,.T.);
#10481=EDGE_CURVE('',#8188,#8187,#4759,.T.);
#10482=EDGE_CURVE('',#8189,#8187,#4760,.T.);
#10483=EDGE_CURVE('',#8190,#8188,#4761,.T.);
#10484=EDGE_CURVE('',#8190,#8189,#4762,.T.);
#10485=EDGE_CURVE('',#8191,#8189,#4763,.T.);
#10486=EDGE_CURVE('',#8192,#8190,#4764,.T.);
#10487=EDGE_CURVE('',#8192,#8191,#4765,.T.);
#10488=EDGE_CURVE('',#8193,#8191,#4766,.T.);
#10489=EDGE_CURVE('',#8194,#8192,#4767,.T.);
#10490=EDGE_CURVE('',#8194,#8193,#4768,.T.);
#10491=EDGE_CURVE('',#8195,#8193,#4769,.T.);
#10492=EDGE_CURVE('',#8196,#8194,#4770,.T.);
#10493=EDGE_CURVE('',#8196,#8195,#4771,.T.);
#10494=EDGE_CURVE('',#8197,#8195,#4772,.T.);
#10495=EDGE_CURVE('',#8198,#8196,#4773,.T.);
#10496=EDGE_CURVE('',#8198,#8197,#4774,.T.);
#10497=EDGE_CURVE('',#8199,#8197,#4775,.T.);
#10498=EDGE_CURVE('',#8200,#8198,#4776,.T.);
#10499=EDGE_CURVE('',#8200,#8199,#4777,.T.);
#10500=EDGE_CURVE('',#8201,#8199,#4778,.T.);
#10501=EDGE_CURVE('',#8202,#8200,#4779,.T.);
#10502=EDGE_CURVE('',#8202,#8201,#4780,.T.);
#10503=EDGE_CURVE('',#8203,#8201,#4781,.T.);
#10504=EDGE_CURVE('',#8204,#8202,#4782,.T.);
#10505=EDGE_CURVE('',#8204,#8203,#4783,.T.);
#10506=EDGE_CURVE('',#8205,#8203,#4784,.T.);
#10507=EDGE_CURVE('',#8206,#8204,#4785,.T.);
#10508=EDGE_CURVE('',#8206,#8205,#4786,.T.);
#10509=EDGE_CURVE('',#8207,#8205,#4787,.T.);
#10510=EDGE_CURVE('',#8208,#8206,#4788,.T.);
#10511=EDGE_CURVE('',#8208,#8207,#4789,.T.);
#10512=EDGE_CURVE('',#8209,#8207,#4790,.T.);
#10513=EDGE_CURVE('',#8210,#8208,#4791,.T.);
#10514=EDGE_CURVE('',#8210,#8209,#4792,.T.);
#10515=EDGE_CURVE('',#8211,#8209,#4793,.T.);
#10516=EDGE_CURVE('',#8212,#8210,#4794,.T.);
#10517=EDGE_CURVE('',#8212,#8211,#4795,.T.);
#10518=EDGE_CURVE('',#8213,#8211,#4796,.T.);
#10519=EDGE_CURVE('',#8214,#8212,#4797,.T.);
#10520=EDGE_CURVE('',#8214,#8213,#4798,.T.);
#10521=EDGE_CURVE('',#8215,#8213,#4799,.T.);
#10522=EDGE_CURVE('',#8216,#8214,#4800,.T.);
#10523=EDGE_CURVE('',#8216,#8215,#4801,.T.);
#10524=EDGE_CURVE('',#8217,#8215,#4802,.T.);
#10525=EDGE_CURVE('',#8218,#8216,#4803,.T.);
#10526=EDGE_CURVE('',#8218,#8217,#4804,.T.);
#10527=EDGE_CURVE('',#8219,#8217,#4805,.T.);
#10528=EDGE_CURVE('',#8220,#8218,#4806,.T.);
#10529=EDGE_CURVE('',#8220,#8219,#4807,.T.);
#10530=EDGE_CURVE('',#8221,#8219,#4808,.T.);
#10531=EDGE_CURVE('',#8222,#8220,#4809,.T.);
#10532=EDGE_CURVE('',#8222,#8221,#4810,.T.);
#10533=EDGE_CURVE('',#8223,#8221,#4811,.T.);
#10534=EDGE_CURVE('',#8224,#8222,#4812,.T.);
#10535=EDGE_CURVE('',#8224,#8223,#4813,.T.);
#10536=EDGE_CURVE('',#8225,#8223,#4814,.T.);
#10537=EDGE_CURVE('',#8226,#8224,#4815,.T.);
#10538=EDGE_CURVE('',#8226,#8225,#4816,.T.);
#10539=EDGE_CURVE('',#8227,#8225,#4817,.T.);
#10540=EDGE_CURVE('',#8228,#8226,#4818,.T.);
#10541=EDGE_CURVE('',#8228,#8227,#4819,.T.);
#10542=EDGE_CURVE('',#8229,#8227,#4820,.T.);
#10543=EDGE_CURVE('',#8230,#8228,#4821,.T.);
#10544=EDGE_CURVE('',#8230,#8229,#4822,.T.);
#10545=EDGE_CURVE('',#8231,#8229,#4823,.T.);
#10546=EDGE_CURVE('',#8232,#8230,#4824,.T.);
#10547=EDGE_CURVE('',#8232,#8231,#4825,.T.);
#10548=EDGE_CURVE('',#8233,#8231,#4826,.T.);
#10549=EDGE_CURVE('',#8234,#8232,#4827,.T.);
#10550=EDGE_CURVE('',#8234,#8233,#4828,.T.);
#10551=EDGE_CURVE('',#8235,#8233,#4829,.T.);
#10552=EDGE_CURVE('',#8236,#8234,#4830,.T.);
#10553=EDGE_CURVE('',#8236,#8235,#4831,.T.);
#10554=EDGE_CURVE('',#8058,#8235,#4832,.T.);
#10555=EDGE_CURVE('',#8059,#8236,#4833,.T.);
#10556=EDGE_CURVE('',#8237,#8237,#1429,.T.);
#10557=EDGE_CURVE('',#8238,#8238,#1430,.T.);
#10558=EDGE_CURVE('',#8239,#8240,#1431,.T.);
#10559=EDGE_CURVE('',#8240,#8239,#1432,.T.);
#10560=EDGE_CURVE('',#8239,#8237,#4834,.T.);
#10561=EDGE_CURVE('',#7850,#7938,#4835,.T.);
#10562=EDGE_CURVE('',#7886,#7888,#343,.T.);
#10563=EDGE_CURVE('',#7890,#7892,#132,.T.);
#10564=EDGE_CURVE('',#7897,#7894,#4836,.T.);
#10565=EDGE_CURVE('',#7936,#7934,#133,.T.);
#10566=EDGE_CURVE('',#7935,#7933,#134,.T.);
#10567=EDGE_CURVE('',#7937,#8241,#4837,.T.);
#10568=EDGE_CURVE('',#7893,#7898,#4838,.T.);
#10569=EDGE_CURVE('',#7885,#7887,#344,.F.);
#10570=EDGE_CURVE('',#8241,#7852,#135,.T.);
#10571=EDGE_CURVE('',#8241,#7851,#4839,.T.);
#10572=EDGE_CURVE('',#7890,#7891,#1433,.T.);
#10573=EDGE_CURVE('',#7852,#7851,#1434,.T.);
#10574=EDGE_CURVE('',#7891,#8242,#4840,.T.);
#10575=EDGE_CURVE('',#8242,#8242,#1435,.T.);
#10576=EDGE_CURVE('',#7851,#8243,#4841,.T.);
#10577=EDGE_CURVE('',#8243,#8243,#1436,.T.);
#10578=EDGE_CURVE('',#8240,#8244,#4842,.T.);
#10579=EDGE_CURVE('',#8244,#8244,#1437,.T.);
#10580=EDGE_CURVE('',#8245,#8245,#1438,.T.);
#10581=EDGE_CURVE('',#8245,#8246,#4843,.T.);
#10582=EDGE_CURVE('',#8246,#8246,#1439,.T.);
#10583=EDGE_CURVE('',#8238,#8245,#4844,.T.);
#10584=EDGE_CURVE('',#8247,#8247,#430,.T.);
#10585=EDGE_CURVE('',#8247,#8248,#4845,.T.);
#10586=EDGE_CURVE('',#8248,#8248,#1440,.T.);
#10587=EDGE_CURVE('',#8249,#8250,#4846,.T.);
#10588=EDGE_CURVE('',#8250,#8251,#1441,.T.);
#10589=EDGE_CURVE('',#8251,#8249,#1442,.T.);
#10590=EDGE_CURVE('',#8249,#8250,#431,.T.);
#10591=EDGE_CURVE('',#8251,#8252,#4847,.T.);
#10592=EDGE_CURVE('',#8252,#8252,#1443,.T.);
#10593=EDGE_CURVE('',#8253,#8254,#4848,.T.);
#10594=EDGE_CURVE('',#8255,#8253,#4849,.T.);
#10595=EDGE_CURVE('',#8256,#8255,#4850,.T.);
#10596=EDGE_CURVE('',#8257,#8256,#4851,.T.);
#10597=EDGE_CURVE('',#8258,#8257,#4852,.T.);
#10598=EDGE_CURVE('',#8254,#8258,#4853,.T.);
#10599=EDGE_CURVE('',#8259,#8260,#4854,.T.);
#10600=EDGE_CURVE('',#8255,#8259,#4855,.T.);
#10601=EDGE_CURVE('',#8253,#8260,#4856,.T.);
#10602=EDGE_CURVE('',#8261,#8259,#4857,.T.);
#10603=EDGE_CURVE('',#8256,#8261,#4858,.T.);
#10604=EDGE_CURVE('',#8262,#8261,#4859,.T.);
#10605=EDGE_CURVE('',#8257,#8262,#4860,.T.);
#10606=EDGE_CURVE('',#8263,#8262,#4861,.T.);
#10607=EDGE_CURVE('',#8258,#8263,#4862,.T.);
#10608=EDGE_CURVE('',#8264,#8263,#4863,.T.);
#10609=EDGE_CURVE('',#8254,#8264,#4864,.T.);
#10610=EDGE_CURVE('',#8260,#8264,#4865,.T.);
#10611=EDGE_CURVE('',#8265,#8266,#345,.T.);
#10612=EDGE_CURVE('',#8267,#8265,#346,.T.);
#10613=EDGE_CURVE('',#8268,#8267,#347,.T.);
#10614=EDGE_CURVE('',#8269,#8268,#4866,.T.);
#10615=EDGE_CURVE('',#8270,#8269,#4867,.T.);
#10616=EDGE_CURVE('',#8271,#8270,#4868,.T.);
#10617=EDGE_CURVE('',#8272,#8271,#4869,.T.);
#10618=EDGE_CURVE('',#8273,#8272,#4870,.T.);
#10619=EDGE_CURVE('',#8274,#8273,#348,.T.);
#10620=EDGE_CURVE('',#8275,#8274,#349,.T.);
#10621=EDGE_CURVE('',#8276,#8275,#350,.T.);
#10622=EDGE_CURVE('',#8266,#8276,#4871,.T.);
#10623=EDGE_CURVE('',#8277,#8278,#351,.T.);
#10624=EDGE_CURVE('',#8267,#8277,#4872,.T.);
#10625=EDGE_CURVE('',#8265,#8278,#4873,.T.);
#10626=EDGE_CURVE('',#8279,#8277,#352,.T.);
#10627=EDGE_CURVE('',#8268,#8279,#4874,.T.);
#10628=EDGE_CURVE('',#8280,#8279,#4875,.T.);
#10629=EDGE_CURVE('',#8269,#8280,#4876,.T.);
#10630=EDGE_CURVE('',#8281,#8280,#4877,.T.);
#10631=EDGE_CURVE('',#8270,#8281,#4878,.T.);
#10632=EDGE_CURVE('',#8282,#8281,#4879,.T.);
#10633=EDGE_CURVE('',#8271,#8282,#4880,.T.);
#10634=EDGE_CURVE('',#8283,#8282,#4881,.T.);
#10635=EDGE_CURVE('',#8272,#8283,#4882,.T.);
#10636=EDGE_CURVE('',#8284,#8283,#4883,.T.);
#10637=EDGE_CURVE('',#8273,#8284,#4884,.T.);
#10638=EDGE_CURVE('',#8285,#8284,#353,.T.);
#10639=EDGE_CURVE('',#8274,#8285,#4885,.T.);
#10640=EDGE_CURVE('',#8286,#8285,#354,.T.);
#10641=EDGE_CURVE('',#8275,#8286,#4886,.T.);
#10642=EDGE_CURVE('',#8287,#8286,#355,.T.);
#10643=EDGE_CURVE('',#8276,#8287,#4887,.T.);
#10644=EDGE_CURVE('',#8288,#8287,#4888,.T.);
#10645=EDGE_CURVE('',#8266,#8288,#4889,.T.);
#10646=EDGE_CURVE('',#8278,#8288,#356,.T.);
#10647=EDGE_CURVE('',#8289,#8290,#4890,.T.);
#10648=EDGE_CURVE('',#8291,#8289,#4891,.T.);
#10649=EDGE_CURVE('',#8291,#8292,#4892,.T.);
#10650=EDGE_CURVE('',#8292,#8293,#4893,.T.);
#10651=EDGE_CURVE('',#8290,#8293,#4894,.T.);
#10652=EDGE_CURVE('',#8294,#8295,#4895,.T.);
#10653=EDGE_CURVE('',#8289,#8294,#4896,.T.);
#10654=EDGE_CURVE('',#8295,#8290,#4897,.T.);
#10655=EDGE_CURVE('',#8296,#8297,#4898,.T.);
#10656=EDGE_CURVE('',#8294,#8296,#4899,.T.);
#10657=EDGE_CURVE('',#8297,#8295,#4900,.T.);
#10658=EDGE_CURVE('',#8298,#8299,#4901,.T.);
#10659=EDGE_CURVE('',#8300,#8298,#4902,.T.);
#10660=EDGE_CURVE('',#8300,#8301,#4903,.T.);
#10661=EDGE_CURVE('',#8299,#8301,#4904,.T.);
#10662=EDGE_CURVE('',#8302,#8303,#4905,.T.);
#10663=EDGE_CURVE('',#8298,#8302,#4906,.T.);
#10664=EDGE_CURVE('',#8303,#8299,#4907,.T.);
#10665=EDGE_CURVE('',#8304,#8305,#4908,.T.);
#10666=EDGE_CURVE('',#8306,#8305,#4909,.T.);
#10667=EDGE_CURVE('',#8302,#8306,#4910,.T.);
#10668=EDGE_CURVE('',#8304,#8303,#4911,.T.);
#10669=EDGE_CURVE('',#8307,#8308,#4912,.T.);
#10670=EDGE_CURVE('',#8309,#8307,#4913,.T.);
#10671=EDGE_CURVE('',#8310,#8309,#4914,.T.);
#10672=EDGE_CURVE('',#8308,#8310,#4915,.T.);
#10673=EDGE_CURVE('',#8311,#8312,#4916,.T.);
#10674=EDGE_CURVE('',#8313,#8312,#4917,.T.);
#10675=EDGE_CURVE('',#8314,#8313,#4918,.T.);
#10676=EDGE_CURVE('',#8307,#8314,#4919,.T.);
#10677=EDGE_CURVE('',#8311,#8308,#4920,.T.);
#10678=EDGE_CURVE('',#8315,#8315,#1444,.T.);
#10679=EDGE_CURVE('',#8316,#8316,#1445,.T.);
#10680=EDGE_CURVE('',#8317,#8317,#1446,.T.);
#10681=EDGE_CURVE('',#8317,#8315,#4921,.T.);
#10682=EDGE_CURVE('',#8318,#8318,#1447,.T.);
#10683=EDGE_CURVE('',#8318,#8316,#4922,.T.);
#10684=EDGE_CURVE('',#8319,#8320,#4923,.T.);
#10685=EDGE_CURVE('',#8320,#8321,#4924,.T.);
#10686=EDGE_CURVE('',#8321,#8322,#4925,.T.);
#10687=EDGE_CURVE('',#8323,#8322,#4926,.T.);
#10688=EDGE_CURVE('',#8324,#8323,#4927,.T.);
#10689=EDGE_CURVE('',#8324,#8319,#4928,.T.);
#10690=EDGE_CURVE('',#8325,#8319,#4929,.T.);
#10691=EDGE_CURVE('',#8326,#8324,#4930,.T.);
#10692=EDGE_CURVE('',#8326,#8325,#4931,.T.);
#10693=EDGE_CURVE('',#8327,#8328,#4932,.T.);
#10694=EDGE_CURVE('',#8328,#8329,#4933,.T.);
#10695=EDGE_CURVE('',#8329,#8325,#4934,.T.);
#10696=EDGE_CURVE('',#8330,#8326,#4935,.T.);
#10697=EDGE_CURVE('',#8330,#8327,#4936,.T.);
#10698=EDGE_CURVE('',#8322,#8327,#4937,.T.);
#10699=EDGE_CURVE('',#8323,#8330,#4938,.T.);
#10700=EDGE_CURVE('',#8321,#8328,#4939,.T.);
#10701=EDGE_CURVE('',#8329,#8320,#4940,.T.);
#10702=EDGE_CURVE('',#8331,#8332,#4941,.T.);
#10703=EDGE_CURVE('',#8333,#8331,#4942,.T.);
#10704=EDGE_CURVE('',#8334,#8333,#4943,.T.);
#10705=EDGE_CURVE('',#8332,#8334,#4944,.T.);
#10706=EDGE_CURVE('',#8335,#8335,#1448,.T.);
#10707=EDGE_CURVE('',#8336,#8336,#1449,.T.);
#10708=EDGE_CURVE('',#8337,#8338,#4945,.T.);
#10709=EDGE_CURVE('',#8338,#8339,#4946,.T.);
#10710=EDGE_CURVE('',#8339,#8340,#4947,.T.);
#10711=EDGE_CURVE('',#8340,#8337,#4948,.T.);
#10712=EDGE_CURVE('',#8341,#8341,#1450,.T.);
#10713=EDGE_CURVE('',#8342,#8342,#1451,.T.);
#10714=EDGE_CURVE('',#8337,#8329,#4949,.T.);
#10715=EDGE_CURVE('',#8340,#8333,#4950,.T.);
#10716=EDGE_CURVE('',#8320,#8331,#4951,.T.);
#10717=EDGE_CURVE('',#8342,#8336,#4952,.T.);
#10718=EDGE_CURVE('',#8341,#8335,#4953,.T.);
#10719=EDGE_CURVE('',#8339,#8334,#4954,.T.);
#10720=EDGE_CURVE('',#8343,#8344,#4955,.T.);
#10721=EDGE_CURVE('',#8343,#8345,#4956,.T.);
#10722=EDGE_CURVE('',#8345,#8332,#4957,.T.);
#10723=EDGE_CURVE('',#8338,#8346,#4958,.T.);
#10724=EDGE_CURVE('',#8344,#8346,#4959,.T.);
#10725=EDGE_CURVE('',#8346,#8345,#4960,.T.);
#10726=EDGE_CURVE('',#8347,#8347,#1452,.T.);
#10727=EDGE_CURVE('',#8348,#8348,#1453,.T.);
#10728=EDGE_CURVE('',#8349,#8349,#1454,.T.);
#10729=EDGE_CURVE('',#8349,#8347,#4961,.T.);
#10730=EDGE_CURVE('',#8350,#8350,#1455,.T.);
#10731=EDGE_CURVE('',#8350,#8348,#4962,.T.);
#10732=EDGE_CURVE('',#8346,#8351,#4963,.T.);
#10733=EDGE_CURVE('',#8351,#8352,#4964,.T.);
#10734=EDGE_CURVE('',#8353,#8352,#4965,.T.);
#10735=EDGE_CURVE('',#8354,#8353,#4966,.T.);
#10736=EDGE_CURVE('',#8354,#8344,#4967,.T.);
#10737=EDGE_CURVE('',#8355,#8354,#4968,.T.);
#10738=EDGE_CURVE('',#8355,#8343,#4969,.T.);
#10739=EDGE_CURVE('',#8356,#8357,#4970,.T.);
#10740=EDGE_CURVE('',#8357,#8345,#4971,.T.);
#10741=EDGE_CURVE('',#8358,#8355,#4972,.T.);
#10742=EDGE_CURVE('',#8358,#8356,#4973,.T.);
#10743=EDGE_CURVE('',#8352,#8356,#4974,.T.);
#10744=EDGE_CURVE('',#8353,#8358,#4975,.T.);
#10745=EDGE_CURVE('',#8310,#8359,#4976,.T.);
#10746=EDGE_CURVE('',#8360,#8309,#4977,.T.);
#10747=EDGE_CURVE('',#8359,#8360,#4978,.T.);
#10748=EDGE_CURVE('',#8361,#8362,#4979,.T.);
#10749=EDGE_CURVE('',#8362,#8363,#4980,.T.);
#10750=EDGE_CURVE('',#8363,#8364,#4981,.T.);
#10751=EDGE_CURVE('',#8364,#8365,#4982,.T.);
#10752=EDGE_CURVE('',#8365,#8366,#4983,.T.);
#10753=EDGE_CURVE('',#8366,#8361,#4984,.T.);
#10754=EDGE_CURVE('',#8321,#8313,#4985,.T.);
#10755=EDGE_CURVE('',#8361,#8312,#4986,.T.);
#10756=EDGE_CURVE('',#8366,#8328,#4987,.T.);
#10757=EDGE_CURVE('',#8357,#8314,#4988,.T.);
#10758=EDGE_CURVE('',#8365,#8351,#4989,.T.);
#10759=EDGE_CURVE('',#8351,#8357,#4990,.T.);
#10760=EDGE_CURVE('',#8364,#8300,#4991,.T.);
#10761=EDGE_CURVE('',#8306,#8291,#4992,.T.);
#10762=EDGE_CURVE('',#8296,#8360,#4993,.T.);
#10763=EDGE_CURVE('',#8297,#8359,#4994,.T.);
#10764=EDGE_CURVE('',#8293,#8311,#4995,.T.);
#10765=EDGE_CURVE('',#8305,#8292,#4996,.T.);
#10766=EDGE_CURVE('',#8362,#8304,#4997,.T.);
#10767=EDGE_CURVE('',#8363,#8301,#4998,.T.);
#10768=EDGE_CURVE('',#8367,#8367,#1456,.T.);
#10769=EDGE_CURVE('',#8368,#8368,#1457,.T.);
#10770=EDGE_CURVE('',#8369,#8370,#1458,.T.);
#10771=EDGE_CURVE('',#8370,#8369,#1459,.T.);
#10772=EDGE_CURVE('',#8370,#8368,#4999,.T.);
#10773=EDGE_CURVE('',#8367,#8369,#5000,.T.);
#10774=EDGE_CURVE('',#8371,#8372,#5001,.T.);
#10775=EDGE_CURVE('',#8372,#8373,#5002,.T.);
#10776=EDGE_CURVE('',#8373,#8374,#1460,.T.);
#10777=EDGE_CURVE('',#8371,#8374,#357,.T.);
#10778=EDGE_CURVE('',#8375,#8376,#5003,.T.);
#10779=EDGE_CURVE('',#8376,#8372,#358,.F.);
#10780=EDGE_CURVE('',#8375,#8371,#359,.T.);
#10781=EDGE_CURVE('',#8377,#8378,#5004,.T.);
#10782=EDGE_CURVE('',#8378,#8376,#360,.F.);
#10783=EDGE_CURVE('',#8377,#8375,#361,.T.);
#10784=EDGE_CURVE('',#8379,#8380,#5005,.T.);
#10785=EDGE_CURVE('',#8380,#8378,#362,.F.);
#10786=EDGE_CURVE('',#8379,#8377,#363,.T.);
#10787=EDGE_CURVE('',#8381,#8382,#5006,.T.);
#10788=EDGE_CURVE('',#8382,#8380,#364,.F.);
#10789=EDGE_CURVE('',#8381,#8379,#365,.T.);
#10790=EDGE_CURVE('',#8383,#8384,#5007,.T.);
#10791=EDGE_CURVE('',#8384,#8382,#366,.F.);
#10792=EDGE_CURVE('',#8383,#8381,#367,.T.);
#10793=EDGE_CURVE('',#8385,#8386,#5008,.T.);
#10794=EDGE_CURVE('',#8386,#8384,#368,.F.);
#10795=EDGE_CURVE('',#8385,#8383,#369,.T.);
#10796=EDGE_CURVE('',#8387,#8388,#5009,.T.);
#10797=EDGE_CURVE('',#8388,#8386,#370,.F.);
#10798=EDGE_CURVE('',#8387,#8385,#371,.T.);
#10799=EDGE_CURVE('',#8389,#8390,#5010,.T.);
#10800=EDGE_CURVE('',#8390,#8388,#372,.F.);
#10801=EDGE_CURVE('',#8389,#8387,#373,.T.);
#10802=EDGE_CURVE('',#8391,#8392,#5011,.T.);
#10803=EDGE_CURVE('',#8392,#8390,#374,.F.);
#10804=EDGE_CURVE('',#8391,#8389,#375,.T.);
#10805=EDGE_CURVE('',#8393,#8394,#5012,.T.);
#10806=EDGE_CURVE('',#8394,#8392,#376,.F.);
#10807=EDGE_CURVE('',#8393,#8391,#377,.T.);
#10808=EDGE_CURVE('',#8395,#8396,#5013,.T.);
#10809=EDGE_CURVE('',#8396,#8394,#378,.F.);
#10810=EDGE_CURVE('',#8395,#8393,#379,.T.);
#10811=EDGE_CURVE('',#8397,#8398,#5014,.T.);
#10812=EDGE_CURVE('',#8398,#8396,#380,.F.);
#10813=EDGE_CURVE('',#8397,#8395,#381,.T.);
#10814=EDGE_CURVE('',#8399,#8400,#5015,.T.);
#10815=EDGE_CURVE('',#8399,#8401,#1461,.T.);
#10816=EDGE_CURVE('',#8401,#8400,#382,.F.);
#10817=EDGE_CURVE('',#8402,#8403,#5016,.T.);
#10818=EDGE_CURVE('',#8403,#8404,#136,.T.);
#10819=EDGE_CURVE('',#8404,#8405,#5017,.T.);
#10820=EDGE_CURVE('',#8402,#8405,#137,.T.);
#10821=EDGE_CURVE('',#8406,#8407,#5018,.T.);
#10822=EDGE_CURVE('',#8407,#8403,#138,.T.);
#10823=EDGE_CURVE('',#8406,#8402,#139,.T.);
#10824=EDGE_CURVE('',#8408,#8409,#5019,.T.);
#10825=EDGE_CURVE('',#8409,#8407,#140,.T.);
#10826=EDGE_CURVE('',#8408,#8406,#141,.T.);
#10827=EDGE_CURVE('',#8410,#8411,#5020,.T.);
#10828=EDGE_CURVE('',#8411,#8409,#142,.T.);
#10829=EDGE_CURVE('',#8410,#8408,#143,.T.);
#10830=EDGE_CURVE('',#8412,#8413,#5021,.T.);
#10831=EDGE_CURVE('',#8413,#8411,#144,.T.);
#10832=EDGE_CURVE('',#8412,#8410,#145,.T.);
#10833=EDGE_CURVE('',#8414,#8415,#5022,.T.);
#10834=EDGE_CURVE('',#8415,#8413,#146,.T.);
#10835=EDGE_CURVE('',#8414,#8412,#147,.T.);
#10836=EDGE_CURVE('',#8416,#8417,#5023,.T.);
#10837=EDGE_CURVE('',#8417,#8415,#148,.T.);
#10838=EDGE_CURVE('',#8416,#8414,#149,.T.);
#10839=EDGE_CURVE('',#8418,#8419,#5024,.T.);
#10840=EDGE_CURVE('',#8419,#8417,#150,.T.);
#10841=EDGE_CURVE('',#8418,#8416,#151,.T.);
#10842=EDGE_CURVE('',#8420,#8421,#5025,.T.);
#10843=EDGE_CURVE('',#8421,#8419,#152,.T.);
#10844=EDGE_CURVE('',#8420,#8418,#153,.T.);
#10845=EDGE_CURVE('',#8422,#8423,#5026,.T.);
#10846=EDGE_CURVE('',#8423,#8421,#154,.T.);
#10847=EDGE_CURVE('',#8422,#8420,#155,.T.);
#10848=EDGE_CURVE('',#8424,#8425,#5027,.T.);
#10849=EDGE_CURVE('',#8425,#8423,#156,.T.);
#10850=EDGE_CURVE('',#8424,#8422,#157,.T.);
#10851=EDGE_CURVE('',#8426,#8427,#5028,.T.);
#10852=EDGE_CURVE('',#8427,#8425,#158,.T.);
#10853=EDGE_CURVE('',#8426,#8424,#159,.T.);
#10854=EDGE_CURVE('',#8428,#8429,#5029,.T.);
#10855=EDGE_CURVE('',#8429,#8427,#160,.T.);
#10856=EDGE_CURVE('',#8428,#8426,#161,.T.);
#10857=EDGE_CURVE('',#8430,#8431,#5030,.T.);
#10858=EDGE_CURVE('',#8432,#8430,#162,.T.);
#10859=EDGE_CURVE('',#8432,#8433,#5031,.T.);
#10860=EDGE_CURVE('',#8433,#8431,#163,.T.);
#10861=EDGE_CURVE('',#8434,#8434,#1462,.T.);
#10862=EDGE_CURVE('',#8434,#8435,#5032,.T.);
#10863=EDGE_CURVE('',#8435,#8435,#1463,.T.);
#10864=EDGE_CURVE('',#8436,#8436,#1464,.T.);
#10865=EDGE_CURVE('',#8436,#8437,#5033,.T.);
#10866=EDGE_CURVE('',#8437,#8437,#1465,.T.);
#10867=EDGE_CURVE('',#8438,#8438,#1466,.T.);
#10868=EDGE_CURVE('',#8438,#8439,#5034,.T.);
#10869=EDGE_CURVE('',#8439,#8439,#1467,.T.);
#10870=EDGE_CURVE('',#8440,#8440,#1468,.T.);
#10871=EDGE_CURVE('',#8440,#8441,#1469,.T.);
#10872=EDGE_CURVE('',#8442,#8441,#1470,.T.);
#10873=EDGE_CURVE('',#8441,#8442,#1471,.T.);
#10874=EDGE_CURVE('',#8443,#8444,#1472,.T.);
#10875=EDGE_CURVE('',#8444,#8443,#1473,.T.);
#10876=EDGE_CURVE('',#8444,#8445,#1474,.T.);
#10877=EDGE_CURVE('',#8445,#8445,#1475,.T.);
#10878=EDGE_CURVE('',#8446,#8447,#1476,.T.);
#10879=EDGE_CURVE('',#8447,#8446,#1477,.T.);
#10880=EDGE_CURVE('',#8447,#8448,#1478,.T.);
#10881=EDGE_CURVE('',#8448,#8448,#1479,.T.);
#10882=EDGE_CURVE('',#8449,#8449,#1480,.T.);
#10883=EDGE_CURVE('',#8449,#8450,#1481,.T.);
#10884=EDGE_CURVE('',#8451,#8450,#1482,.T.);
#10885=EDGE_CURVE('',#8450,#8451,#1483,.T.);
#10886=EDGE_CURVE('',#8446,#8451,#5035,.T.);
#10887=EDGE_CURVE('',#8443,#8442,#5036,.T.);
#10888=EDGE_CURVE('',#8452,#8452,#1484,.T.);
#10889=EDGE_CURVE('',#8453,#8453,#1485,.T.);
#10890=EDGE_CURVE('',#8454,#8401,#164,.T.);
#10891=EDGE_CURVE('',#8401,#8455,#1486,.T.);
#10892=EDGE_CURVE('',#8455,#8399,#1487,.T.);
#10893=EDGE_CURVE('',#8399,#8454,#5037,.T.);
#10894=EDGE_CURVE('',#8454,#8432,#5038,.T.);
#10895=EDGE_CURVE('',#8430,#8428,#165,.T.);
#10896=EDGE_CURVE('',#8405,#8372,#5039,.T.);
#10897=EDGE_CURVE('',#8400,#8398,#383,.F.);
#10898=EDGE_CURVE('',#8431,#8429,#166,.T.);
#10899=EDGE_CURVE('',#8433,#8399,#5040,.T.);
#10900=EDGE_CURVE('',#8399,#8397,#384,.T.);
#10901=EDGE_CURVE('',#8374,#8456,#167,.T.);
#10902=EDGE_CURVE('',#8456,#8404,#5041,.T.);
#10903=EDGE_CURVE('',#8373,#8456,#5042,.T.);
#10904=EDGE_CURVE('',#8374,#8373,#1488,.T.);
#10905=EDGE_CURVE('',#8455,#8457,#5043,.T.);
#10906=EDGE_CURVE('',#8457,#8457,#1489,.T.);
#10907=EDGE_CURVE('',#8373,#8453,#5044,.T.);
#10908=EDGE_CURVE('',#8458,#8459,#1490,.T.);
#10909=EDGE_CURVE('',#8459,#8458,#1491,.T.);
#10910=EDGE_CURVE('',#8459,#8460,#5045,.T.);
#10911=EDGE_CURVE('',#8460,#8460,#1492,.T.);
#10912=EDGE_CURVE('',#8461,#8461,#1493,.T.);
#10913=EDGE_CURVE('',#8461,#8462,#1494,.T.);
#10914=EDGE_CURVE('',#8462,#8462,#1495,.T.);
#10915=EDGE_CURVE('',#8463,#8463,#1496,.T.);
#10916=EDGE_CURVE('',#8463,#8464,#1497,.T.);
#10917=EDGE_CURVE('',#8464,#8464,#1498,.T.);
#10918=EDGE_CURVE('',#8464,#8461,#5046,.T.);
#10919=EDGE_CURVE('',#8465,#8465,#1499,.T.);
#10920=EDGE_CURVE('',#8465,#8452,#5047,.T.);
#10921=EDGE_CURVE('',#8466,#8467,#1500,.T.);
#10922=EDGE_CURVE('',#8466,#8468,#5048,.T.);
#10923=EDGE_CURVE('',#8469,#8468,#1501,.T.);
#10924=EDGE_CURVE('',#8467,#8469,#5049,.T.);
#10925=EDGE_CURVE('',#8470,#8470,#1502,.T.);
#10926=EDGE_CURVE('',#8470,#8471,#5050,.T.);
#10927=EDGE_CURVE('',#8471,#8471,#1503,.T.);
#10928=EDGE_CURVE('',#8472,#8473,#5051,.T.);
#10929=EDGE_CURVE('',#8473,#8474,#5052,.T.);
#10930=EDGE_CURVE('',#8474,#8475,#5053,.T.);
#10931=EDGE_CURVE('',#8475,#8476,#5054,.T.);
#10932=EDGE_CURVE('',#8476,#8477,#5055,.T.);
#10933=EDGE_CURVE('',#8477,#8478,#5056,.T.);
#10934=EDGE_CURVE('',#8478,#8479,#5057,.T.);
#10935=EDGE_CURVE('',#8479,#8480,#1504,.T.);
#10936=EDGE_CURVE('',#8480,#8481,#5058,.T.);
#10937=EDGE_CURVE('',#8481,#8482,#5059,.T.);
#10938=EDGE_CURVE('',#8482,#8483,#5060,.T.);
#10939=EDGE_CURVE('',#8483,#8484,#5061,.T.);
#10940=EDGE_CURVE('',#8484,#8485,#5062,.T.);
#10941=EDGE_CURVE('',#8485,#8472,#5063,.T.);
#10942=EDGE_CURVE('',#8486,#8487,#1505,.T.);
#10943=EDGE_CURVE('',#8486,#8488,#5064,.T.);
#10944=EDGE_CURVE('',#8489,#8488,#1506,.T.);
#10945=EDGE_CURVE('',#8487,#8489,#5065,.T.);
#10946=EDGE_CURVE('',#8490,#8491,#5066,.T.);
#10947=EDGE_CURVE('',#8490,#8492,#5067,.T.);
#10948=EDGE_CURVE('',#8493,#8492,#5068,.T.);
#10949=EDGE_CURVE('',#8494,#8493,#5069,.T.);
#10950=EDGE_CURVE('',#8494,#8495,#5070,.T.);
#10951=EDGE_CURVE('',#8496,#8495,#5071,.T.);
#10952=EDGE_CURVE('',#8497,#8496,#5072,.T.);
#10953=EDGE_CURVE('',#8498,#8497,#5073,.T.);
#10954=EDGE_CURVE('',#8499,#8498,#5074,.T.);
#10955=EDGE_CURVE('',#8500,#8499,#1507,.T.);
#10956=EDGE_CURVE('',#8501,#8500,#5075,.T.);
#10957=EDGE_CURVE('',#8502,#8501,#5076,.T.);
#10958=EDGE_CURVE('',#8503,#8502,#5077,.T.);
#10959=EDGE_CURVE('',#8491,#8503,#5078,.T.);
#10960=EDGE_CURVE('',#8504,#8504,#1508,.T.);
#10961=EDGE_CURVE('',#8505,#8506,#5079,.T.);
#10962=EDGE_CURVE('',#8507,#8505,#5080,.T.);
#10963=EDGE_CURVE('',#8508,#8507,#5081,.T.);
#10964=EDGE_CURVE('',#8509,#8508,#5082,.T.);
#10965=EDGE_CURVE('',#8510,#8509,#5083,.T.);
#10966=EDGE_CURVE('',#8506,#8510,#5084,.T.);
#10967=EDGE_CURVE('',#8511,#8489,#5085,.T.);
#10968=EDGE_CURVE('',#8511,#8512,#1509,.T.);
#10969=EDGE_CURVE('',#8512,#8513,#5086,.T.);
#10970=EDGE_CURVE('',#8513,#8490,#1510,.T.);
#10971=EDGE_CURVE('',#8475,#8491,#5087,.T.);
#10972=EDGE_CURVE('',#8474,#8514,#1511,.T.);
#10973=EDGE_CURVE('',#8515,#8514,#5088,.T.);
#10974=EDGE_CURVE('',#8515,#8516,#1512,.T.);
#10975=EDGE_CURVE('',#8487,#8516,#5089,.T.);
#10976=EDGE_CURVE('',#8476,#8503,#5090,.T.);
#10977=EDGE_CURVE('',#8477,#8502,#5091,.T.);
#10978=EDGE_CURVE('',#8478,#8501,#5092,.T.);
#10979=EDGE_CURVE('',#8479,#8500,#5093,.T.);
#10980=EDGE_CURVE('',#8480,#8499,#5094,.T.);
#10981=EDGE_CURVE('',#8481,#8498,#5095,.T.);
#10982=EDGE_CURVE('',#8482,#8497,#5096,.T.);
#10983=EDGE_CURVE('',#8483,#8496,#5097,.T.);
#10984=EDGE_CURVE('',#8495,#8517,#432,.T.);
#10985=EDGE_CURVE('',#8518,#8517,#5098,.T.);
#10986=EDGE_CURVE('',#8518,#8519,#433,.T.);
#10987=EDGE_CURVE('',#8468,#8519,#5099,.T.);
#10988=EDGE_CURVE('',#8520,#8466,#5100,.T.);
#10989=EDGE_CURVE('',#8520,#8521,#434,.T.);
#10990=EDGE_CURVE('',#8521,#8522,#5101,.T.);
#10991=EDGE_CURVE('',#8522,#8484,#435,.T.);
#10992=EDGE_CURVE('',#8523,#8524,#5102,.T.);
#10993=EDGE_CURVE('',#8524,#8494,#436,.T.);
#10994=EDGE_CURVE('',#8472,#8493,#5103,.T.);
#10995=EDGE_CURVE('',#8485,#8525,#437,.T.);
#10996=EDGE_CURVE('',#8526,#8525,#5104,.T.);
#10997=EDGE_CURVE('',#8526,#8527,#438,.T.);
#10998=EDGE_CURVE('',#8467,#8527,#5105,.T.);
#10999=EDGE_CURVE('',#8528,#8469,#5106,.T.);
#11000=EDGE_CURVE('',#8528,#8523,#439,.T.);
#11001=EDGE_CURVE('',#8529,#8530,#5107,.T.);
#11002=EDGE_CURVE('',#8529,#8531,#440,.T.);
#11003=EDGE_CURVE('',#8488,#8531,#5108,.T.);
#11004=EDGE_CURVE('',#8532,#8486,#5109,.T.);
#11005=EDGE_CURVE('',#8532,#8533,#441,.T.);
#11006=EDGE_CURVE('',#8533,#8534,#5110,.T.);
#11007=EDGE_CURVE('',#8534,#8473,#442,.T.);
#11008=EDGE_CURVE('',#8492,#8530,#443,.T.);
#11009=EDGE_CURVE('',#8527,#8520,#5111,.T.);
#11010=EDGE_CURVE('',#8525,#8522,#5112,.T.);
#11011=EDGE_CURVE('',#8521,#8526,#5113,.T.);
#11012=EDGE_CURVE('',#8523,#8518,#5114,.T.);
#11013=EDGE_CURVE('',#8517,#8524,#5115,.T.);
#11014=EDGE_CURVE('',#8519,#8528,#5116,.T.);
#11015=EDGE_CURVE('',#8531,#8511,#5117,.T.);
#11016=EDGE_CURVE('',#8512,#8529,#5118,.T.);
#11017=EDGE_CURVE('',#8530,#8513,#5119,.T.);
#11018=EDGE_CURVE('',#8533,#8515,#5120,.T.);
#11019=EDGE_CURVE('',#8514,#8534,#5121,.T.);
#11020=EDGE_CURVE('',#8516,#8532,#5122,.T.);
#11021=EDGE_CURVE('',#8505,#8535,#5123,.T.);
#11022=EDGE_CURVE('',#8535,#8536,#5124,.T.);
#11023=EDGE_CURVE('',#8507,#8536,#5125,.T.);
#11024=EDGE_CURVE('',#8506,#8537,#5126,.T.);
#11025=EDGE_CURVE('',#8537,#8535,#5127,.T.);
#11026=EDGE_CURVE('',#8510,#8538,#5128,.T.);
#11027=EDGE_CURVE('',#8538,#8537,#5129,.T.);
#11028=EDGE_CURVE('',#8509,#8539,#5130,.T.);
#11029=EDGE_CURVE('',#8539,#8538,#5131,.T.);
#11030=EDGE_CURVE('',#8508,#8540,#5132,.T.);
#11031=EDGE_CURVE('',#8540,#8539,#5133,.T.);
#11032=EDGE_CURVE('',#8536,#8540,#5134,.T.);
#11033=EDGE_CURVE('',#8541,#8542,#5135,.T.);
#11034=EDGE_CURVE('',#8542,#8543,#5136,.T.);
#11035=EDGE_CURVE('',#8543,#8544,#5137,.T.);
#11036=EDGE_CURVE('',#8544,#8545,#5138,.T.);
#11037=EDGE_CURVE('',#8545,#8546,#5139,.T.);
#11038=EDGE_CURVE('',#8546,#8541,#5140,.T.);
#11039=EDGE_CURVE('',#8535,#8545,#444,.T.);
#11040=EDGE_CURVE('',#8546,#8537,#445,.T.);
#11041=EDGE_CURVE('',#8541,#8538,#446,.T.);
#11042=EDGE_CURVE('',#8536,#8544,#447,.T.);
#11043=EDGE_CURVE('',#8542,#8539,#448,.T.);
#11044=EDGE_CURVE('',#8540,#8543,#449,.T.);
#11045=EDGE_CURVE('',#8458,#8504,#5141,.T.);
#11046=EDGE_CURVE('',#8547,#8547,#1513,.T.);
#11047=EDGE_CURVE('',#8547,#8548,#5142,.T.);
#11048=EDGE_CURVE('',#8548,#8548,#1514,.T.);
#11049=EDGE_CURVE('',#8549,#8550,#5143,.T.);
#11050=EDGE_CURVE('',#8551,#8550,#5144,.T.);
#11051=EDGE_CURVE('',#8552,#8551,#5145,.T.);
#11052=EDGE_CURVE('',#8552,#8549,#5146,.T.);
#11053=EDGE_CURVE('',#8553,#8552,#1515,.T.);
#11054=EDGE_CURVE('',#8553,#8554,#5147,.T.);
#11055=EDGE_CURVE('',#8554,#8549,#1516,.T.);
#11056=EDGE_CURVE('',#8555,#8554,#5148,.T.);
#11057=EDGE_CURVE('',#8556,#8553,#5149,.T.);
#11058=EDGE_CURVE('',#8556,#8555,#5150,.T.);
#11059=EDGE_CURVE('',#8557,#8555,#5151,.T.);
#11060=EDGE_CURVE('',#8558,#8556,#5152,.T.);
#11061=EDGE_CURVE('',#8558,#8557,#5153,.T.);
#11062=EDGE_CURVE('',#8559,#8557,#5154,.T.);
#11063=EDGE_CURVE('',#8560,#8558,#5155,.T.);
#11064=EDGE_CURVE('',#8560,#8559,#5156,.T.);
#11065=EDGE_CURVE('',#8561,#8559,#5157,.T.);
#11066=EDGE_CURVE('',#8562,#8560,#5158,.T.);
#11067=EDGE_CURVE('',#8562,#8561,#5159,.T.);
#11068=EDGE_CURVE('',#8563,#8561,#5160,.T.);
#11069=EDGE_CURVE('',#8564,#8562,#5161,.T.);
#11070=EDGE_CURVE('',#8564,#8563,#5162,.T.);
#11071=EDGE_CURVE('',#8565,#8563,#5163,.T.);
#11072=EDGE_CURVE('',#8566,#8564,#5164,.T.);
#11073=EDGE_CURVE('',#8566,#8565,#5165,.T.);
#11074=EDGE_CURVE('',#8567,#8565,#5166,.T.);
#11075=EDGE_CURVE('',#8568,#8566,#5167,.T.);
#11076=EDGE_CURVE('',#8568,#8567,#5168,.T.);
#11077=EDGE_CURVE('',#8569,#8567,#5169,.T.);
#11078=EDGE_CURVE('',#8570,#8568,#5170,.T.);
#11079=EDGE_CURVE('',#8570,#8569,#5171,.T.);
#11080=EDGE_CURVE('',#8571,#8569,#5172,.T.);
#11081=EDGE_CURVE('',#8572,#8570,#5173,.T.);
#11082=EDGE_CURVE('',#8572,#8571,#5174,.T.);
#11083=EDGE_CURVE('',#8573,#8571,#5175,.T.);
#11084=EDGE_CURVE('',#8574,#8572,#5176,.T.);
#11085=EDGE_CURVE('',#8574,#8573,#5177,.T.);
#11086=EDGE_CURVE('',#8575,#8573,#5178,.T.);
#11087=EDGE_CURVE('',#8576,#8574,#5179,.T.);
#11088=EDGE_CURVE('',#8576,#8575,#5180,.T.);
#11089=EDGE_CURVE('',#8577,#8575,#5181,.T.);
#11090=EDGE_CURVE('',#8578,#8576,#5182,.T.);
#11091=EDGE_CURVE('',#8578,#8577,#5183,.T.);
#11092=EDGE_CURVE('',#8579,#8577,#5184,.T.);
#11093=EDGE_CURVE('',#8580,#8578,#5185,.T.);
#11094=EDGE_CURVE('',#8580,#8579,#5186,.T.);
#11095=EDGE_CURVE('',#8581,#8579,#5187,.T.);
#11096=EDGE_CURVE('',#8582,#8580,#5188,.T.);
#11097=EDGE_CURVE('',#8582,#8581,#5189,.T.);
#11098=EDGE_CURVE('',#8583,#8581,#5190,.T.);
#11099=EDGE_CURVE('',#8584,#8582,#5191,.T.);
#11100=EDGE_CURVE('',#8584,#8583,#5192,.T.);
#11101=EDGE_CURVE('',#8585,#8583,#5193,.T.);
#11102=EDGE_CURVE('',#8586,#8584,#5194,.T.);
#11103=EDGE_CURVE('',#8586,#8585,#5195,.T.);
#11104=EDGE_CURVE('',#8587,#8585,#5196,.T.);
#11105=EDGE_CURVE('',#8588,#8586,#5197,.T.);
#11106=EDGE_CURVE('',#8588,#8587,#5198,.T.);
#11107=EDGE_CURVE('',#8589,#8587,#5199,.T.);
#11108=EDGE_CURVE('',#8590,#8588,#5200,.T.);
#11109=EDGE_CURVE('',#8590,#8589,#5201,.T.);
#11110=EDGE_CURVE('',#8591,#8589,#5202,.T.);
#11111=EDGE_CURVE('',#8592,#8590,#5203,.T.);
#11112=EDGE_CURVE('',#8592,#8591,#5204,.T.);
#11113=EDGE_CURVE('',#8593,#8591,#5205,.T.);
#11114=EDGE_CURVE('',#8594,#8592,#5206,.T.);
#11115=EDGE_CURVE('',#8594,#8593,#5207,.T.);
#11116=EDGE_CURVE('',#8595,#8593,#5208,.T.);
#11117=EDGE_CURVE('',#8596,#8594,#5209,.T.);
#11118=EDGE_CURVE('',#8596,#8595,#5210,.T.);
#11119=EDGE_CURVE('',#8597,#8595,#5211,.T.);
#11120=EDGE_CURVE('',#8598,#8596,#5212,.T.);
#11121=EDGE_CURVE('',#8598,#8597,#5213,.T.);
#11122=EDGE_CURVE('',#8599,#8597,#5214,.T.);
#11123=EDGE_CURVE('',#8600,#8598,#5215,.T.);
#11124=EDGE_CURVE('',#8600,#8599,#5216,.T.);
#11125=EDGE_CURVE('',#8601,#8599,#5217,.T.);
#11126=EDGE_CURVE('',#8602,#8600,#5218,.T.);
#11127=EDGE_CURVE('',#8602,#8601,#5219,.T.);
#11128=EDGE_CURVE('',#8603,#8601,#5220,.T.);
#11129=EDGE_CURVE('',#8604,#8602,#5221,.T.);
#11130=EDGE_CURVE('',#8604,#8603,#5222,.T.);
#11131=EDGE_CURVE('',#8605,#8603,#5223,.T.);
#11132=EDGE_CURVE('',#8606,#8604,#5224,.T.);
#11133=EDGE_CURVE('',#8606,#8605,#5225,.T.);
#11134=EDGE_CURVE('',#8607,#8605,#5226,.T.);
#11135=EDGE_CURVE('',#8608,#8606,#5227,.T.);
#11136=EDGE_CURVE('',#8608,#8607,#5228,.T.);
#11137=EDGE_CURVE('',#8609,#8607,#5229,.T.);
#11138=EDGE_CURVE('',#8610,#8608,#5230,.T.);
#11139=EDGE_CURVE('',#8610,#8609,#5231,.T.);
#11140=EDGE_CURVE('',#8611,#8609,#5232,.T.);
#11141=EDGE_CURVE('',#8612,#8610,#5233,.T.);
#11142=EDGE_CURVE('',#8612,#8611,#5234,.T.);
#11143=EDGE_CURVE('',#8613,#8611,#5235,.T.);
#11144=EDGE_CURVE('',#8614,#8612,#5236,.T.);
#11145=EDGE_CURVE('',#8614,#8613,#5237,.T.);
#11146=EDGE_CURVE('',#8615,#8613,#5238,.T.);
#11147=EDGE_CURVE('',#8616,#8614,#5239,.T.);
#11148=EDGE_CURVE('',#8616,#8615,#5240,.T.);
#11149=EDGE_CURVE('',#8617,#8615,#5241,.T.);
#11150=EDGE_CURVE('',#8618,#8616,#5242,.T.);
#11151=EDGE_CURVE('',#8618,#8617,#5243,.T.);
#11152=EDGE_CURVE('',#8619,#8617,#5244,.T.);
#11153=EDGE_CURVE('',#8620,#8618,#5245,.T.);
#11154=EDGE_CURVE('',#8620,#8619,#5246,.T.);
#11155=EDGE_CURVE('',#8621,#8619,#5247,.T.);
#11156=EDGE_CURVE('',#8622,#8620,#5248,.T.);
#11157=EDGE_CURVE('',#8622,#8621,#5249,.T.);
#11158=EDGE_CURVE('',#8623,#8621,#5250,.T.);
#11159=EDGE_CURVE('',#8624,#8622,#5251,.T.);
#11160=EDGE_CURVE('',#8624,#8623,#5252,.T.);
#11161=EDGE_CURVE('',#8625,#8623,#5253,.T.);
#11162=EDGE_CURVE('',#8626,#8624,#5254,.T.);
#11163=EDGE_CURVE('',#8626,#8625,#5255,.T.);
#11164=EDGE_CURVE('',#8627,#8625,#5256,.T.);
#11165=EDGE_CURVE('',#8628,#8626,#5257,.T.);
#11166=EDGE_CURVE('',#8628,#8627,#5258,.T.);
#11167=EDGE_CURVE('',#8629,#8627,#5259,.T.);
#11168=EDGE_CURVE('',#8630,#8628,#5260,.T.);
#11169=EDGE_CURVE('',#8630,#8629,#5261,.T.);
#11170=EDGE_CURVE('',#8631,#8629,#1517,.T.);
#11171=EDGE_CURVE('',#8632,#8630,#1518,.T.);
#11172=EDGE_CURVE('',#8632,#8631,#5262,.T.);
#11173=EDGE_CURVE('',#8633,#8631,#5263,.T.);
#11174=EDGE_CURVE('',#8634,#8632,#5264,.T.);
#11175=EDGE_CURVE('',#8634,#8633,#5265,.T.);
#11176=EDGE_CURVE('',#8550,#8633,#5266,.T.);
#11177=EDGE_CURVE('',#8551,#8634,#5267,.T.);
#11178=EDGE_CURVE('',#8635,#8635,#1519,.T.);
#11179=EDGE_CURVE('',#8635,#8636,#5268,.T.);
#11180=EDGE_CURVE('',#8636,#8636,#1520,.T.);
#11181=EDGE_CURVE('',#8637,#8638,#5269,.T.);
#11182=EDGE_CURVE('',#8639,#8638,#5270,.T.);
#11183=EDGE_CURVE('',#8640,#8639,#5271,.T.);
#11184=EDGE_CURVE('',#8640,#8637,#5272,.T.);
#11185=EDGE_CURVE('',#8641,#8640,#1521,.T.);
#11186=EDGE_CURVE('',#8641,#8642,#5273,.T.);
#11187=EDGE_CURVE('',#8642,#8637,#1522,.T.);
#11188=EDGE_CURVE('',#8643,#8642,#5274,.T.);
#11189=EDGE_CURVE('',#8644,#8641,#5275,.T.);
#11190=EDGE_CURVE('',#8644,#8643,#5276,.T.);
#11191=EDGE_CURVE('',#8645,#8643,#5277,.T.);
#11192=EDGE_CURVE('',#8646,#8644,#5278,.T.);
#11193=EDGE_CURVE('',#8646,#8645,#5279,.T.);
#11194=EDGE_CURVE('',#8647,#8645,#5280,.T.);
#11195=EDGE_CURVE('',#8648,#8646,#5281,.T.);
#11196=EDGE_CURVE('',#8648,#8647,#5282,.T.);
#11197=EDGE_CURVE('',#8649,#8647,#5283,.T.);
#11198=EDGE_CURVE('',#8650,#8648,#5284,.T.);
#11199=EDGE_CURVE('',#8650,#8649,#5285,.T.);
#11200=EDGE_CURVE('',#8651,#8649,#1523,.T.);
#11201=EDGE_CURVE('',#8652,#8650,#1524,.T.);
#11202=EDGE_CURVE('',#8652,#8651,#5286,.T.);
#11203=EDGE_CURVE('',#8653,#8651,#5287,.T.);
#11204=EDGE_CURVE('',#8654,#8652,#5288,.T.);
#11205=EDGE_CURVE('',#8654,#8653,#5289,.T.);
#11206=EDGE_CURVE('',#8655,#8653,#5290,.T.);
#11207=EDGE_CURVE('',#8656,#8654,#5291,.T.);
#11208=EDGE_CURVE('',#8656,#8655,#5292,.T.);
#11209=EDGE_CURVE('',#8657,#8655,#5293,.T.);
#11210=EDGE_CURVE('',#8658,#8656,#5294,.T.);
#11211=EDGE_CURVE('',#8658,#8657,#5295,.T.);
#11212=EDGE_CURVE('',#8638,#8657,#1525,.T.);
#11213=EDGE_CURVE('',#8639,#8658,#1526,.T.);
#11214=ORIENTED_EDGE('',*,*,#8659,.F.);
#11215=ORIENTED_EDGE('',*,*,#8660,.T.);
#11216=ORIENTED_EDGE('',*,*,#8661,.F.);
#11217=ORIENTED_EDGE('',*,*,#8662,.F.);
#11218=ORIENTED_EDGE('',*,*,#8663,.T.);
#11219=ORIENTED_EDGE('',*,*,#8664,.T.);
#11220=ORIENTED_EDGE('',*,*,#8665,.T.);
#11221=ORIENTED_EDGE('',*,*,#8666,.T.);
#11222=ORIENTED_EDGE('',*,*,#8667,.T.);
#11223=ORIENTED_EDGE('',*,*,#8668,.T.);
#11224=ORIENTED_EDGE('',*,*,#8669,.T.);
#11225=ORIENTED_EDGE('',*,*,#8670,.T.);
#11226=ORIENTED_EDGE('',*,*,#8671,.T.);
#11227=ORIENTED_EDGE('',*,*,#8672,.T.);
#11228=ORIENTED_EDGE('',*,*,#8673,.T.);
#11229=ORIENTED_EDGE('',*,*,#8674,.T.);
#11230=ORIENTED_EDGE('',*,*,#8675,.T.);
#11231=ORIENTED_EDGE('',*,*,#8676,.T.);
#11232=ORIENTED_EDGE('',*,*,#8677,.T.);
#11233=ORIENTED_EDGE('',*,*,#8678,.T.);
#11234=ORIENTED_EDGE('',*,*,#8679,.T.);
#11235=ORIENTED_EDGE('',*,*,#8680,.T.);
#11236=ORIENTED_EDGE('',*,*,#8681,.T.);
#11237=ORIENTED_EDGE('',*,*,#8682,.T.);
#11238=ORIENTED_EDGE('',*,*,#8683,.T.);
#11239=ORIENTED_EDGE('',*,*,#8684,.T.);
#11240=ORIENTED_EDGE('',*,*,#8685,.T.);
#11241=ORIENTED_EDGE('',*,*,#8686,.T.);
#11242=ORIENTED_EDGE('',*,*,#8687,.T.);
#11243=ORIENTED_EDGE('',*,*,#8688,.T.);
#11244=ORIENTED_EDGE('',*,*,#8689,.T.);
#11245=ORIENTED_EDGE('',*,*,#8690,.T.);
#11246=ORIENTED_EDGE('',*,*,#8691,.F.);
#11247=ORIENTED_EDGE('',*,*,#8692,.F.);
#11248=ORIENTED_EDGE('',*,*,#8693,.T.);
#11249=ORIENTED_EDGE('',*,*,#8694,.T.);
#11250=ORIENTED_EDGE('',*,*,#8695,.F.);
#11251=ORIENTED_EDGE('',*,*,#8696,.F.);
#11252=ORIENTED_EDGE('',*,*,#8697,.T.);
#11253=ORIENTED_EDGE('',*,*,#8698,.T.);
#11254=ORIENTED_EDGE('',*,*,#8699,.F.);
#11255=ORIENTED_EDGE('',*,*,#8700,.F.);
#11256=ORIENTED_EDGE('',*,*,#8701,.T.);
#11257=ORIENTED_EDGE('',*,*,#8702,.T.);
#11258=ORIENTED_EDGE('',*,*,#8703,.F.);
#11259=ORIENTED_EDGE('',*,*,#8704,.F.);
#11260=ORIENTED_EDGE('',*,*,#8705,.T.);
#11261=ORIENTED_EDGE('',*,*,#8706,.T.);
#11262=ORIENTED_EDGE('',*,*,#8707,.F.);
#11263=ORIENTED_EDGE('',*,*,#8708,.F.);
#11264=ORIENTED_EDGE('',*,*,#8709,.T.);
#11265=ORIENTED_EDGE('',*,*,#8710,.T.);
#11266=ORIENTED_EDGE('',*,*,#8711,.F.);
#11267=ORIENTED_EDGE('',*,*,#8712,.F.);
#11268=ORIENTED_EDGE('',*,*,#8713,.T.);
#11269=ORIENTED_EDGE('',*,*,#8714,.T.);
#11270=ORIENTED_EDGE('',*,*,#8715,.F.);
#11271=ORIENTED_EDGE('',*,*,#8716,.F.);
#11272=ORIENTED_EDGE('',*,*,#8717,.T.);
#11273=ORIENTED_EDGE('',*,*,#8718,.T.);
#11274=ORIENTED_EDGE('',*,*,#8719,.F.);
#11275=ORIENTED_EDGE('',*,*,#8720,.F.);
#11276=ORIENTED_EDGE('',*,*,#8721,.T.);
#11277=ORIENTED_EDGE('',*,*,#8722,.T.);
#11278=ORIENTED_EDGE('',*,*,#8723,.F.);
#11279=ORIENTED_EDGE('',*,*,#8724,.F.);
#11280=ORIENTED_EDGE('',*,*,#8725,.T.);
#11281=ORIENTED_EDGE('',*,*,#8726,.T.);
#11282=ORIENTED_EDGE('',*,*,#8727,.F.);
#11283=ORIENTED_EDGE('',*,*,#8728,.F.);
#11284=ORIENTED_EDGE('',*,*,#8729,.T.);
#11285=ORIENTED_EDGE('',*,*,#8730,.T.);
#11286=ORIENTED_EDGE('',*,*,#8731,.F.);
#11287=ORIENTED_EDGE('',*,*,#8732,.F.);
#11288=ORIENTED_EDGE('',*,*,#8733,.T.);
#11289=ORIENTED_EDGE('',*,*,#8734,.T.);
#11290=ORIENTED_EDGE('',*,*,#8735,.F.);
#11291=ORIENTED_EDGE('',*,*,#8736,.F.);
#11292=ORIENTED_EDGE('',*,*,#8737,.T.);
#11293=ORIENTED_EDGE('',*,*,#8738,.T.);
#11294=ORIENTED_EDGE('',*,*,#8739,.F.);
#11295=ORIENTED_EDGE('',*,*,#8740,.F.);
#11296=ORIENTED_EDGE('',*,*,#8741,.T.);
#11297=ORIENTED_EDGE('',*,*,#8742,.T.);
#11298=ORIENTED_EDGE('',*,*,#8743,.F.);
#11299=ORIENTED_EDGE('',*,*,#8744,.F.);
#11300=ORIENTED_EDGE('',*,*,#8745,.T.);
#11301=ORIENTED_EDGE('',*,*,#8746,.T.);
#11302=ORIENTED_EDGE('',*,*,#8747,.F.);
#11303=ORIENTED_EDGE('',*,*,#8748,.F.);
#11304=ORIENTED_EDGE('',*,*,#8749,.T.);
#11305=ORIENTED_EDGE('',*,*,#8750,.T.);
#11306=ORIENTED_EDGE('',*,*,#8751,.F.);
#11307=ORIENTED_EDGE('',*,*,#8752,.F.);
#11308=ORIENTED_EDGE('',*,*,#8753,.T.);
#11309=ORIENTED_EDGE('',*,*,#8754,.T.);
#11310=ORIENTED_EDGE('',*,*,#8755,.F.);
#11311=ORIENTED_EDGE('',*,*,#8756,.F.);
#11312=ORIENTED_EDGE('',*,*,#8757,.T.);
#11313=ORIENTED_EDGE('',*,*,#8758,.T.);
#11314=ORIENTED_EDGE('',*,*,#8759,.F.);
#11315=ORIENTED_EDGE('',*,*,#8760,.F.);
#11316=ORIENTED_EDGE('',*,*,#8761,.T.);
#11317=ORIENTED_EDGE('',*,*,#8762,.T.);
#11318=ORIENTED_EDGE('',*,*,#8763,.F.);
#11319=ORIENTED_EDGE('',*,*,#8764,.F.);
#11320=ORIENTED_EDGE('',*,*,#8765,.T.);
#11321=ORIENTED_EDGE('',*,*,#8766,.T.);
#11322=ORIENTED_EDGE('',*,*,#8767,.F.);
#11323=ORIENTED_EDGE('',*,*,#8768,.F.);
#11324=ORIENTED_EDGE('',*,*,#8769,.T.);
#11325=ORIENTED_EDGE('',*,*,#8770,.T.);
#11326=ORIENTED_EDGE('',*,*,#8771,.F.);
#11327=ORIENTED_EDGE('',*,*,#8772,.F.);
#11328=ORIENTED_EDGE('',*,*,#8773,.T.);
#11329=ORIENTED_EDGE('',*,*,#8774,.T.);
#11330=ORIENTED_EDGE('',*,*,#8775,.F.);
#11331=ORIENTED_EDGE('',*,*,#8776,.F.);
#11332=ORIENTED_EDGE('',*,*,#8777,.T.);
#11333=ORIENTED_EDGE('',*,*,#8778,.T.);
#11334=ORIENTED_EDGE('',*,*,#8779,.F.);
#11335=ORIENTED_EDGE('',*,*,#8780,.F.);
#11336=ORIENTED_EDGE('',*,*,#8781,.T.);
#11337=ORIENTED_EDGE('',*,*,#8782,.T.);
#11338=ORIENTED_EDGE('',*,*,#8783,.F.);
#11339=ORIENTED_EDGE('',*,*,#8784,.F.);
#11340=ORIENTED_EDGE('',*,*,#8785,.T.);
#11341=ORIENTED_EDGE('',*,*,#8786,.T.);
#11342=ORIENTED_EDGE('',*,*,#8787,.F.);
#11343=ORIENTED_EDGE('',*,*,#8788,.F.);
#11344=ORIENTED_EDGE('',*,*,#8789,.T.);
#11345=ORIENTED_EDGE('',*,*,#8790,.T.);
#11346=ORIENTED_EDGE('',*,*,#8791,.F.);
#11347=ORIENTED_EDGE('',*,*,#8792,.F.);
#11348=ORIENTED_EDGE('',*,*,#8793,.F.);
#11349=ORIENTED_EDGE('',*,*,#8794,.T.);
#11350=ORIENTED_EDGE('',*,*,#8795,.T.);
#11351=ORIENTED_EDGE('',*,*,#8796,.F.);
#11352=ORIENTED_EDGE('',*,*,#8797,.F.);
#11353=ORIENTED_EDGE('',*,*,#8798,.T.);
#11354=ORIENTED_EDGE('',*,*,#8799,.T.);
#11355=ORIENTED_EDGE('',*,*,#8800,.F.);
#11356=ORIENTED_EDGE('',*,*,#8801,.F.);
#11357=ORIENTED_EDGE('',*,*,#8802,.T.);
#11358=ORIENTED_EDGE('',*,*,#8803,.T.);
#11359=ORIENTED_EDGE('',*,*,#8804,.F.);
#11360=ORIENTED_EDGE('',*,*,#8805,.F.);
#11361=ORIENTED_EDGE('',*,*,#8806,.T.);
#11362=ORIENTED_EDGE('',*,*,#8807,.T.);
#11363=ORIENTED_EDGE('',*,*,#8808,.F.);
#11364=ORIENTED_EDGE('',*,*,#8809,.F.);
#11365=ORIENTED_EDGE('',*,*,#8810,.T.);
#11366=ORIENTED_EDGE('',*,*,#8811,.T.);
#11367=ORIENTED_EDGE('',*,*,#8812,.F.);
#11368=ORIENTED_EDGE('',*,*,#8813,.F.);
#11369=ORIENTED_EDGE('',*,*,#8814,.T.);
#11370=ORIENTED_EDGE('',*,*,#8815,.T.);
#11371=ORIENTED_EDGE('',*,*,#8816,.F.);
#11372=ORIENTED_EDGE('',*,*,#8817,.F.);
#11373=ORIENTED_EDGE('',*,*,#8818,.T.);
#11374=ORIENTED_EDGE('',*,*,#8819,.T.);
#11375=ORIENTED_EDGE('',*,*,#8820,.F.);
#11376=ORIENTED_EDGE('',*,*,#8821,.F.);
#11377=ORIENTED_EDGE('',*,*,#8822,.T.);
#11378=ORIENTED_EDGE('',*,*,#8823,.T.);
#11379=ORIENTED_EDGE('',*,*,#8824,.F.);
#11380=ORIENTED_EDGE('',*,*,#8825,.F.);
#11381=ORIENTED_EDGE('',*,*,#8826,.T.);
#11382=ORIENTED_EDGE('',*,*,#8827,.T.);
#11383=ORIENTED_EDGE('',*,*,#8828,.F.);
#11384=ORIENTED_EDGE('',*,*,#8829,.F.);
#11385=ORIENTED_EDGE('',*,*,#8830,.T.);
#11386=ORIENTED_EDGE('',*,*,#8831,.T.);
#11387=ORIENTED_EDGE('',*,*,#8832,.F.);
#11388=ORIENTED_EDGE('',*,*,#8833,.F.);
#11389=ORIENTED_EDGE('',*,*,#8834,.T.);
#11390=ORIENTED_EDGE('',*,*,#8835,.T.);
#11391=ORIENTED_EDGE('',*,*,#8836,.F.);
#11392=ORIENTED_EDGE('',*,*,#8837,.F.);
#11393=ORIENTED_EDGE('',*,*,#8838,.T.);
#11394=ORIENTED_EDGE('',*,*,#8839,.T.);
#11395=ORIENTED_EDGE('',*,*,#8840,.F.);
#11396=ORIENTED_EDGE('',*,*,#8841,.F.);
#11397=ORIENTED_EDGE('',*,*,#8842,.T.);
#11398=ORIENTED_EDGE('',*,*,#8843,.T.);
#11399=ORIENTED_EDGE('',*,*,#8844,.F.);
#11400=ORIENTED_EDGE('',*,*,#8845,.F.);
#11401=ORIENTED_EDGE('',*,*,#8846,.T.);
#11402=ORIENTED_EDGE('',*,*,#8847,.T.);
#11403=ORIENTED_EDGE('',*,*,#8848,.F.);
#11404=ORIENTED_EDGE('',*,*,#8849,.F.);
#11405=ORIENTED_EDGE('',*,*,#8850,.T.);
#11406=ORIENTED_EDGE('',*,*,#8851,.T.);
#11407=ORIENTED_EDGE('',*,*,#8852,.F.);
#11408=ORIENTED_EDGE('',*,*,#8853,.F.);
#11409=ORIENTED_EDGE('',*,*,#8854,.T.);
#11410=ORIENTED_EDGE('',*,*,#8855,.T.);
#11411=ORIENTED_EDGE('',*,*,#8856,.F.);
#11412=ORIENTED_EDGE('',*,*,#8857,.F.);
#11413=ORIENTED_EDGE('',*,*,#8858,.T.);
#11414=ORIENTED_EDGE('',*,*,#8859,.T.);
#11415=ORIENTED_EDGE('',*,*,#8860,.F.);
#11416=ORIENTED_EDGE('',*,*,#8861,.F.);
#11417=ORIENTED_EDGE('',*,*,#8862,.T.);
#11418=ORIENTED_EDGE('',*,*,#8863,.T.);
#11419=ORIENTED_EDGE('',*,*,#8864,.F.);
#11420=ORIENTED_EDGE('',*,*,#8865,.F.);
#11421=ORIENTED_EDGE('',*,*,#8866,.T.);
#11422=ORIENTED_EDGE('',*,*,#8867,.T.);
#11423=ORIENTED_EDGE('',*,*,#8868,.F.);
#11424=ORIENTED_EDGE('',*,*,#8869,.F.);
#11425=ORIENTED_EDGE('',*,*,#8870,.T.);
#11426=ORIENTED_EDGE('',*,*,#8871,.T.);
#11427=ORIENTED_EDGE('',*,*,#8872,.F.);
#11428=ORIENTED_EDGE('',*,*,#8873,.F.);
#11429=ORIENTED_EDGE('',*,*,#8874,.T.);
#11430=ORIENTED_EDGE('',*,*,#8875,.T.);
#11431=ORIENTED_EDGE('',*,*,#8876,.F.);
#11432=ORIENTED_EDGE('',*,*,#8877,.F.);
#11433=ORIENTED_EDGE('',*,*,#8878,.T.);
#11434=ORIENTED_EDGE('',*,*,#8879,.T.);
#11435=ORIENTED_EDGE('',*,*,#8880,.F.);
#11436=ORIENTED_EDGE('',*,*,#8881,.F.);
#11437=ORIENTED_EDGE('',*,*,#8882,.T.);
#11438=ORIENTED_EDGE('',*,*,#8883,.T.);
#11439=ORIENTED_EDGE('',*,*,#8884,.F.);
#11440=ORIENTED_EDGE('',*,*,#8885,.F.);
#11441=ORIENTED_EDGE('',*,*,#8886,.T.);
#11442=ORIENTED_EDGE('',*,*,#8887,.T.);
#11443=ORIENTED_EDGE('',*,*,#8888,.F.);
#11444=ORIENTED_EDGE('',*,*,#8889,.F.);
#11445=ORIENTED_EDGE('',*,*,#8890,.T.);
#11446=ORIENTED_EDGE('',*,*,#8891,.T.);
#11447=ORIENTED_EDGE('',*,*,#8892,.F.);
#11448=ORIENTED_EDGE('',*,*,#8893,.F.);
#11449=ORIENTED_EDGE('',*,*,#8894,.T.);
#11450=ORIENTED_EDGE('',*,*,#8895,.T.);
#11451=ORIENTED_EDGE('',*,*,#8896,.F.);
#11452=ORIENTED_EDGE('',*,*,#8897,.F.);
#11453=ORIENTED_EDGE('',*,*,#8898,.T.);
#11454=ORIENTED_EDGE('',*,*,#8899,.T.);
#11455=ORIENTED_EDGE('',*,*,#8900,.F.);
#11456=ORIENTED_EDGE('',*,*,#8901,.F.);
#11457=ORIENTED_EDGE('',*,*,#8902,.F.);
#11458=ORIENTED_EDGE('',*,*,#8903,.F.);
#11459=ORIENTED_EDGE('',*,*,#8904,.F.);
#11460=ORIENTED_EDGE('',*,*,#8905,.F.);
#11461=ORIENTED_EDGE('',*,*,#8906,.F.);
#11462=ORIENTED_EDGE('',*,*,#8907,.F.);
#11463=ORIENTED_EDGE('',*,*,#8908,.F.);
#11464=ORIENTED_EDGE('',*,*,#8909,.F.);
#11465=ORIENTED_EDGE('',*,*,#8910,.F.);
#11466=ORIENTED_EDGE('',*,*,#8911,.F.);
#11467=ORIENTED_EDGE('',*,*,#8912,.F.);
#11468=ORIENTED_EDGE('',*,*,#8913,.F.);
#11469=ORIENTED_EDGE('',*,*,#8914,.F.);
#11470=ORIENTED_EDGE('',*,*,#8915,.F.);
#11471=ORIENTED_EDGE('',*,*,#8916,.F.);
#11472=ORIENTED_EDGE('',*,*,#8917,.F.);
#11473=ORIENTED_EDGE('',*,*,#8918,.F.);
#11474=ORIENTED_EDGE('',*,*,#8919,.F.);
#11475=ORIENTED_EDGE('',*,*,#8920,.F.);
#11476=ORIENTED_EDGE('',*,*,#8921,.F.);
#11477=ORIENTED_EDGE('',*,*,#8922,.F.);
#11478=ORIENTED_EDGE('',*,*,#8923,.F.);
#11479=ORIENTED_EDGE('',*,*,#8924,.F.);
#11480=ORIENTED_EDGE('',*,*,#8925,.F.);
#11481=ORIENTED_EDGE('',*,*,#8926,.F.);
#11482=ORIENTED_EDGE('',*,*,#8790,.F.);
#11483=ORIENTED_EDGE('',*,*,#8927,.F.);
#11484=ORIENTED_EDGE('',*,*,#8800,.T.);
#11485=ORIENTED_EDGE('',*,*,#8928,.T.);
#11486=ORIENTED_EDGE('',*,*,#8926,.T.);
#11487=ORIENTED_EDGE('',*,*,#8929,.T.);
#11488=ORIENTED_EDGE('',*,*,#8663,.F.);
#11489=ORIENTED_EDGE('',*,*,#8929,.F.);
#11490=ORIENTED_EDGE('',*,*,#8925,.T.);
#11491=ORIENTED_EDGE('',*,*,#8930,.T.);
#11492=ORIENTED_EDGE('',*,*,#8664,.F.);
#11493=ORIENTED_EDGE('',*,*,#8930,.F.);
#11494=ORIENTED_EDGE('',*,*,#8924,.T.);
#11495=ORIENTED_EDGE('',*,*,#8931,.T.);
#11496=ORIENTED_EDGE('',*,*,#8665,.F.);
#11497=ORIENTED_EDGE('',*,*,#8931,.F.);
#11498=ORIENTED_EDGE('',*,*,#8923,.T.);
#11499=ORIENTED_EDGE('',*,*,#8932,.T.);
#11500=ORIENTED_EDGE('',*,*,#8666,.F.);
#11501=ORIENTED_EDGE('',*,*,#8932,.F.);
#11502=ORIENTED_EDGE('',*,*,#8922,.T.);
#11503=ORIENTED_EDGE('',*,*,#8933,.T.);
#11504=ORIENTED_EDGE('',*,*,#8667,.F.);
#11505=ORIENTED_EDGE('',*,*,#8933,.F.);
#11506=ORIENTED_EDGE('',*,*,#8921,.T.);
#11507=ORIENTED_EDGE('',*,*,#8934,.T.);
#11508=ORIENTED_EDGE('',*,*,#8668,.F.);
#11509=ORIENTED_EDGE('',*,*,#8934,.F.);
#11510=ORIENTED_EDGE('',*,*,#8920,.T.);
#11511=ORIENTED_EDGE('',*,*,#8935,.T.);
#11512=ORIENTED_EDGE('',*,*,#8669,.F.);
#11513=ORIENTED_EDGE('',*,*,#8935,.F.);
#11514=ORIENTED_EDGE('',*,*,#8919,.T.);
#11515=ORIENTED_EDGE('',*,*,#8936,.T.);
#11516=ORIENTED_EDGE('',*,*,#8670,.F.);
#11517=ORIENTED_EDGE('',*,*,#8936,.F.);
#11518=ORIENTED_EDGE('',*,*,#8918,.T.);
#11519=ORIENTED_EDGE('',*,*,#8937,.T.);
#11520=ORIENTED_EDGE('',*,*,#8671,.F.);
#11521=ORIENTED_EDGE('',*,*,#8937,.F.);
#11522=ORIENTED_EDGE('',*,*,#8917,.T.);
#11523=ORIENTED_EDGE('',*,*,#8938,.T.);
#11524=ORIENTED_EDGE('',*,*,#8672,.F.);
#11525=ORIENTED_EDGE('',*,*,#8938,.F.);
#11526=ORIENTED_EDGE('',*,*,#8916,.T.);
#11527=ORIENTED_EDGE('',*,*,#8939,.T.);
#11528=ORIENTED_EDGE('',*,*,#8673,.F.);
#11529=ORIENTED_EDGE('',*,*,#8939,.F.);
#11530=ORIENTED_EDGE('',*,*,#8915,.T.);
#11531=ORIENTED_EDGE('',*,*,#8940,.T.);
#11532=ORIENTED_EDGE('',*,*,#8674,.F.);
#11533=ORIENTED_EDGE('',*,*,#8940,.F.);
#11534=ORIENTED_EDGE('',*,*,#8914,.T.);
#11535=ORIENTED_EDGE('',*,*,#8941,.T.);
#11536=ORIENTED_EDGE('',*,*,#8675,.F.);
#11537=ORIENTED_EDGE('',*,*,#8941,.F.);
#11538=ORIENTED_EDGE('',*,*,#8913,.T.);
#11539=ORIENTED_EDGE('',*,*,#8942,.T.);
#11540=ORIENTED_EDGE('',*,*,#8676,.F.);
#11541=ORIENTED_EDGE('',*,*,#8942,.F.);
#11542=ORIENTED_EDGE('',*,*,#8912,.T.);
#11543=ORIENTED_EDGE('',*,*,#8943,.T.);
#11544=ORIENTED_EDGE('',*,*,#8677,.F.);
#11545=ORIENTED_EDGE('',*,*,#8943,.F.);
#11546=ORIENTED_EDGE('',*,*,#8911,.T.);
#11547=ORIENTED_EDGE('',*,*,#8944,.T.);
#11548=ORIENTED_EDGE('',*,*,#8678,.F.);
#11549=ORIENTED_EDGE('',*,*,#8944,.F.);
#11550=ORIENTED_EDGE('',*,*,#8910,.T.);
#11551=ORIENTED_EDGE('',*,*,#8945,.T.);
#11552=ORIENTED_EDGE('',*,*,#8679,.F.);
#11553=ORIENTED_EDGE('',*,*,#8945,.F.);
#11554=ORIENTED_EDGE('',*,*,#8909,.T.);
#11555=ORIENTED_EDGE('',*,*,#8946,.T.);
#11556=ORIENTED_EDGE('',*,*,#8680,.F.);
#11557=ORIENTED_EDGE('',*,*,#8946,.F.);
#11558=ORIENTED_EDGE('',*,*,#8908,.T.);
#11559=ORIENTED_EDGE('',*,*,#8947,.T.);
#11560=ORIENTED_EDGE('',*,*,#8681,.F.);
#11561=ORIENTED_EDGE('',*,*,#8947,.F.);
#11562=ORIENTED_EDGE('',*,*,#8907,.T.);
#11563=ORIENTED_EDGE('',*,*,#8948,.T.);
#11564=ORIENTED_EDGE('',*,*,#8682,.F.);
#11565=ORIENTED_EDGE('',*,*,#8948,.F.);
#11566=ORIENTED_EDGE('',*,*,#8906,.T.);
#11567=ORIENTED_EDGE('',*,*,#8949,.T.);
#11568=ORIENTED_EDGE('',*,*,#8683,.F.);
#11569=ORIENTED_EDGE('',*,*,#8949,.F.);
#11570=ORIENTED_EDGE('',*,*,#8905,.T.);
#11571=ORIENTED_EDGE('',*,*,#8950,.T.);
#11572=ORIENTED_EDGE('',*,*,#8684,.F.);
#11573=ORIENTED_EDGE('',*,*,#8950,.F.);
#11574=ORIENTED_EDGE('',*,*,#8904,.T.);
#11575=ORIENTED_EDGE('',*,*,#8951,.T.);
#11576=ORIENTED_EDGE('',*,*,#8685,.F.);
#11577=ORIENTED_EDGE('',*,*,#8951,.F.);
#11578=ORIENTED_EDGE('',*,*,#8903,.T.);
#11579=ORIENTED_EDGE('',*,*,#8952,.T.);
#11580=ORIENTED_EDGE('',*,*,#8686,.F.);
#11581=ORIENTED_EDGE('',*,*,#8952,.F.);
#11582=ORIENTED_EDGE('',*,*,#8902,.T.);
#11583=ORIENTED_EDGE('',*,*,#8953,.T.);
#11584=ORIENTED_EDGE('',*,*,#8687,.F.);
#11585=ORIENTED_EDGE('',*,*,#8953,.F.);
#11586=ORIENTED_EDGE('',*,*,#8901,.T.);
#11587=ORIENTED_EDGE('',*,*,#8954,.T.);
#11588=ORIENTED_EDGE('',*,*,#8688,.F.);
#11589=ORIENTED_EDGE('',*,*,#8954,.F.);
#11590=ORIENTED_EDGE('',*,*,#8690,.F.);
#11591=ORIENTED_EDGE('',*,*,#8955,.F.);
#11592=ORIENTED_EDGE('',*,*,#8900,.T.);
#11593=ORIENTED_EDGE('',*,*,#8956,.T.);
#11594=ORIENTED_EDGE('',*,*,#8694,.F.);
#11595=ORIENTED_EDGE('',*,*,#8957,.F.);
#11596=ORIENTED_EDGE('',*,*,#8896,.T.);
#11597=ORIENTED_EDGE('',*,*,#8958,.T.);
#11598=ORIENTED_EDGE('',*,*,#8698,.F.);
#11599=ORIENTED_EDGE('',*,*,#8959,.F.);
#11600=ORIENTED_EDGE('',*,*,#8892,.T.);
#11601=ORIENTED_EDGE('',*,*,#8960,.T.);
#11602=ORIENTED_EDGE('',*,*,#8702,.F.);
#11603=ORIENTED_EDGE('',*,*,#8961,.F.);
#11604=ORIENTED_EDGE('',*,*,#8888,.T.);
#11605=ORIENTED_EDGE('',*,*,#8962,.T.);
#11606=ORIENTED_EDGE('',*,*,#8706,.F.);
#11607=ORIENTED_EDGE('',*,*,#8963,.F.);
#11608=ORIENTED_EDGE('',*,*,#8884,.T.);
#11609=ORIENTED_EDGE('',*,*,#8964,.T.);
#11610=ORIENTED_EDGE('',*,*,#8710,.F.);
#11611=ORIENTED_EDGE('',*,*,#8965,.F.);
#11612=ORIENTED_EDGE('',*,*,#8880,.T.);
#11613=ORIENTED_EDGE('',*,*,#8966,.T.);
#11614=ORIENTED_EDGE('',*,*,#8714,.F.);
#11615=ORIENTED_EDGE('',*,*,#8967,.F.);
#11616=ORIENTED_EDGE('',*,*,#8876,.T.);
#11617=ORIENTED_EDGE('',*,*,#8968,.T.);
#11618=ORIENTED_EDGE('',*,*,#8718,.F.);
#11619=ORIENTED_EDGE('',*,*,#8969,.F.);
#11620=ORIENTED_EDGE('',*,*,#8872,.T.);
#11621=ORIENTED_EDGE('',*,*,#8970,.T.);
#11622=ORIENTED_EDGE('',*,*,#8722,.F.);
#11623=ORIENTED_EDGE('',*,*,#8971,.F.);
#11624=ORIENTED_EDGE('',*,*,#8868,.T.);
#11625=ORIENTED_EDGE('',*,*,#8972,.T.);
#11626=ORIENTED_EDGE('',*,*,#8726,.F.);
#11627=ORIENTED_EDGE('',*,*,#8973,.F.);
#11628=ORIENTED_EDGE('',*,*,#8864,.T.);
#11629=ORIENTED_EDGE('',*,*,#8974,.T.);
#11630=ORIENTED_EDGE('',*,*,#8730,.F.);
#11631=ORIENTED_EDGE('',*,*,#8975,.F.);
#11632=ORIENTED_EDGE('',*,*,#8860,.T.);
#11633=ORIENTED_EDGE('',*,*,#8976,.T.);
#11634=ORIENTED_EDGE('',*,*,#8734,.F.);
#11635=ORIENTED_EDGE('',*,*,#8977,.F.);
#11636=ORIENTED_EDGE('',*,*,#8856,.T.);
#11637=ORIENTED_EDGE('',*,*,#8978,.T.);
#11638=ORIENTED_EDGE('',*,*,#8738,.F.);
#11639=ORIENTED_EDGE('',*,*,#8979,.F.);
#11640=ORIENTED_EDGE('',*,*,#8852,.T.);
#11641=ORIENTED_EDGE('',*,*,#8980,.T.);
#11642=ORIENTED_EDGE('',*,*,#8742,.F.);
#11643=ORIENTED_EDGE('',*,*,#8981,.F.);
#11644=ORIENTED_EDGE('',*,*,#8848,.T.);
#11645=ORIENTED_EDGE('',*,*,#8982,.T.);
#11646=ORIENTED_EDGE('',*,*,#8746,.F.);
#11647=ORIENTED_EDGE('',*,*,#8983,.F.);
#11648=ORIENTED_EDGE('',*,*,#8844,.T.);
#11649=ORIENTED_EDGE('',*,*,#8984,.T.);
#11650=ORIENTED_EDGE('',*,*,#8750,.F.);
#11651=ORIENTED_EDGE('',*,*,#8985,.F.);
#11652=ORIENTED_EDGE('',*,*,#8840,.T.);
#11653=ORIENTED_EDGE('',*,*,#8986,.T.);
#11654=ORIENTED_EDGE('',*,*,#8754,.F.);
#11655=ORIENTED_EDGE('',*,*,#8987,.F.);
#11656=ORIENTED_EDGE('',*,*,#8836,.T.);
#11657=ORIENTED_EDGE('',*,*,#8988,.T.);
#11658=ORIENTED_EDGE('',*,*,#8758,.F.);
#11659=ORIENTED_EDGE('',*,*,#8989,.F.);
#11660=ORIENTED_EDGE('',*,*,#8832,.T.);
#11661=ORIENTED_EDGE('',*,*,#8990,.T.);
#11662=ORIENTED_EDGE('',*,*,#8762,.F.);
#11663=ORIENTED_EDGE('',*,*,#8991,.F.);
#11664=ORIENTED_EDGE('',*,*,#8828,.T.);
#11665=ORIENTED_EDGE('',*,*,#8992,.T.);
#11666=ORIENTED_EDGE('',*,*,#8766,.F.);
#11667=ORIENTED_EDGE('',*,*,#8993,.F.);
#11668=ORIENTED_EDGE('',*,*,#8824,.T.);
#11669=ORIENTED_EDGE('',*,*,#8994,.T.);
#11670=ORIENTED_EDGE('',*,*,#8770,.F.);
#11671=ORIENTED_EDGE('',*,*,#8995,.F.);
#11672=ORIENTED_EDGE('',*,*,#8820,.T.);
#11673=ORIENTED_EDGE('',*,*,#8996,.T.);
#11674=ORIENTED_EDGE('',*,*,#8774,.F.);
#11675=ORIENTED_EDGE('',*,*,#8997,.F.);
#11676=ORIENTED_EDGE('',*,*,#8816,.T.);
#11677=ORIENTED_EDGE('',*,*,#8998,.T.);
#11678=ORIENTED_EDGE('',*,*,#8778,.F.);
#11679=ORIENTED_EDGE('',*,*,#8999,.F.);
#11680=ORIENTED_EDGE('',*,*,#8812,.T.);
#11681=ORIENTED_EDGE('',*,*,#9000,.T.);
#11682=ORIENTED_EDGE('',*,*,#8782,.F.);
#11683=ORIENTED_EDGE('',*,*,#9001,.F.);
#11684=ORIENTED_EDGE('',*,*,#8808,.T.);
#11685=ORIENTED_EDGE('',*,*,#9002,.T.);
#11686=ORIENTED_EDGE('',*,*,#8786,.F.);
#11687=ORIENTED_EDGE('',*,*,#9003,.F.);
#11688=ORIENTED_EDGE('',*,*,#8804,.T.);
#11689=ORIENTED_EDGE('',*,*,#9004,.T.);
#11690=ORIENTED_EDGE('',*,*,#9005,.F.);
#11691=ORIENTED_EDGE('',*,*,#8796,.T.);
#11692=ORIENTED_EDGE('',*,*,#9006,.T.);
#11693=ORIENTED_EDGE('',*,*,#8660,.F.);
#11694=ORIENTED_EDGE('',*,*,#8661,.T.);
#11695=ORIENTED_EDGE('',*,*,#9006,.F.);
#11696=ORIENTED_EDGE('',*,*,#8795,.F.);
#11697=ORIENTED_EDGE('',*,*,#9007,.T.);
#11698=ORIENTED_EDGE('',*,*,#8794,.F.);
#11699=ORIENTED_EDGE('',*,*,#9008,.T.);
#11700=ORIENTED_EDGE('',*,*,#8662,.T.);
#11701=ORIENTED_EDGE('',*,*,#9007,.F.);
#11702=ORIENTED_EDGE('',*,*,#8691,.T.);
#11703=ORIENTED_EDGE('',*,*,#8956,.F.);
#11704=ORIENTED_EDGE('',*,*,#8899,.F.);
#11705=ORIENTED_EDGE('',*,*,#9009,.T.);
#11706=ORIENTED_EDGE('',*,*,#8692,.T.);
#11707=ORIENTED_EDGE('',*,*,#9009,.F.);
#11708=ORIENTED_EDGE('',*,*,#8898,.F.);
#11709=ORIENTED_EDGE('',*,*,#9010,.T.);
#11710=ORIENTED_EDGE('',*,*,#8689,.F.);
#11711=ORIENTED_EDGE('',*,*,#9010,.F.);
#11712=ORIENTED_EDGE('',*,*,#8897,.T.);
#11713=ORIENTED_EDGE('',*,*,#8955,.T.);
#11714=ORIENTED_EDGE('',*,*,#8695,.T.);
#11715=ORIENTED_EDGE('',*,*,#8958,.F.);
#11716=ORIENTED_EDGE('',*,*,#8895,.F.);
#11717=ORIENTED_EDGE('',*,*,#9011,.T.);
#11718=ORIENTED_EDGE('',*,*,#8696,.T.);
#11719=ORIENTED_EDGE('',*,*,#9011,.F.);
#11720=ORIENTED_EDGE('',*,*,#8894,.F.);
#11721=ORIENTED_EDGE('',*,*,#9012,.T.);
#11722=ORIENTED_EDGE('',*,*,#8693,.F.);
#11723=ORIENTED_EDGE('',*,*,#9012,.F.);
#11724=ORIENTED_EDGE('',*,*,#8893,.T.);
#11725=ORIENTED_EDGE('',*,*,#8957,.T.);
#11726=ORIENTED_EDGE('',*,*,#8699,.T.);
#11727=ORIENTED_EDGE('',*,*,#8960,.F.);
#11728=ORIENTED_EDGE('',*,*,#8891,.F.);
#11729=ORIENTED_EDGE('',*,*,#9013,.T.);
#11730=ORIENTED_EDGE('',*,*,#8700,.T.);
#11731=ORIENTED_EDGE('',*,*,#9013,.F.);
#11732=ORIENTED_EDGE('',*,*,#8890,.F.);
#11733=ORIENTED_EDGE('',*,*,#9014,.T.);
#11734=ORIENTED_EDGE('',*,*,#8697,.F.);
#11735=ORIENTED_EDGE('',*,*,#9014,.F.);
#11736=ORIENTED_EDGE('',*,*,#8889,.T.);
#11737=ORIENTED_EDGE('',*,*,#8959,.T.);
#11738=ORIENTED_EDGE('',*,*,#8703,.T.);
#11739=ORIENTED_EDGE('',*,*,#8962,.F.);
#11740=ORIENTED_EDGE('',*,*,#8887,.F.);
#11741=ORIENTED_EDGE('',*,*,#9015,.T.);
#11742=ORIENTED_EDGE('',*,*,#8704,.T.);
#11743=ORIENTED_EDGE('',*,*,#9015,.F.);
#11744=ORIENTED_EDGE('',*,*,#8886,.F.);
#11745=ORIENTED_EDGE('',*,*,#9016,.T.);
#11746=ORIENTED_EDGE('',*,*,#8701,.F.);
#11747=ORIENTED_EDGE('',*,*,#9016,.F.);
#11748=ORIENTED_EDGE('',*,*,#8885,.T.);
#11749=ORIENTED_EDGE('',*,*,#8961,.T.);
#11750=ORIENTED_EDGE('',*,*,#8707,.T.);
#11751=ORIENTED_EDGE('',*,*,#8964,.F.);
#11752=ORIENTED_EDGE('',*,*,#8883,.F.);
#11753=ORIENTED_EDGE('',*,*,#9017,.T.);
#11754=ORIENTED_EDGE('',*,*,#8708,.T.);
#11755=ORIENTED_EDGE('',*,*,#9017,.F.);
#11756=ORIENTED_EDGE('',*,*,#8882,.F.);
#11757=ORIENTED_EDGE('',*,*,#9018,.T.);
#11758=ORIENTED_EDGE('',*,*,#8705,.F.);
#11759=ORIENTED_EDGE('',*,*,#9018,.F.);
#11760=ORIENTED_EDGE('',*,*,#8881,.T.);
#11761=ORIENTED_EDGE('',*,*,#8963,.T.);
#11762=ORIENTED_EDGE('',*,*,#8711,.T.);
#11763=ORIENTED_EDGE('',*,*,#8966,.F.);
#11764=ORIENTED_EDGE('',*,*,#8879,.F.);
#11765=ORIENTED_EDGE('',*,*,#9019,.T.);
#11766=ORIENTED_EDGE('',*,*,#8712,.T.);
#11767=ORIENTED_EDGE('',*,*,#9019,.F.);
#11768=ORIENTED_EDGE('',*,*,#8878,.F.);
#11769=ORIENTED_EDGE('',*,*,#9020,.T.);
#11770=ORIENTED_EDGE('',*,*,#8709,.F.);
#11771=ORIENTED_EDGE('',*,*,#9020,.F.);
#11772=ORIENTED_EDGE('',*,*,#8877,.T.);
#11773=ORIENTED_EDGE('',*,*,#8965,.T.);
#11774=ORIENTED_EDGE('',*,*,#8715,.T.);
#11775=ORIENTED_EDGE('',*,*,#8968,.F.);
#11776=ORIENTED_EDGE('',*,*,#8875,.F.);
#11777=ORIENTED_EDGE('',*,*,#9021,.T.);
#11778=ORIENTED_EDGE('',*,*,#8716,.T.);
#11779=ORIENTED_EDGE('',*,*,#9021,.F.);
#11780=ORIENTED_EDGE('',*,*,#8874,.F.);
#11781=ORIENTED_EDGE('',*,*,#9022,.T.);
#11782=ORIENTED_EDGE('',*,*,#8713,.F.);
#11783=ORIENTED_EDGE('',*,*,#9022,.F.);
#11784=ORIENTED_EDGE('',*,*,#8873,.T.);
#11785=ORIENTED_EDGE('',*,*,#8967,.T.);
#11786=ORIENTED_EDGE('',*,*,#8719,.T.);
#11787=ORIENTED_EDGE('',*,*,#8970,.F.);
#11788=ORIENTED_EDGE('',*,*,#8871,.F.);
#11789=ORIENTED_EDGE('',*,*,#9023,.T.);
#11790=ORIENTED_EDGE('',*,*,#8720,.T.);
#11791=ORIENTED_EDGE('',*,*,#9023,.F.);
#11792=ORIENTED_EDGE('',*,*,#8870,.F.);
#11793=ORIENTED_EDGE('',*,*,#9024,.T.);
#11794=ORIENTED_EDGE('',*,*,#8717,.F.);
#11795=ORIENTED_EDGE('',*,*,#9024,.F.);
#11796=ORIENTED_EDGE('',*,*,#8869,.T.);
#11797=ORIENTED_EDGE('',*,*,#8969,.T.);
#11798=ORIENTED_EDGE('',*,*,#8723,.T.);
#11799=ORIENTED_EDGE('',*,*,#8972,.F.);
#11800=ORIENTED_EDGE('',*,*,#8867,.F.);
#11801=ORIENTED_EDGE('',*,*,#9025,.T.);
#11802=ORIENTED_EDGE('',*,*,#8724,.T.);
#11803=ORIENTED_EDGE('',*,*,#9025,.F.);
#11804=ORIENTED_EDGE('',*,*,#8866,.F.);
#11805=ORIENTED_EDGE('',*,*,#9026,.T.);
#11806=ORIENTED_EDGE('',*,*,#8721,.F.);
#11807=ORIENTED_EDGE('',*,*,#9026,.F.);
#11808=ORIENTED_EDGE('',*,*,#8865,.T.);
#11809=ORIENTED_EDGE('',*,*,#8971,.T.);
#11810=ORIENTED_EDGE('',*,*,#8727,.T.);
#11811=ORIENTED_EDGE('',*,*,#8974,.F.);
#11812=ORIENTED_EDGE('',*,*,#8863,.F.);
#11813=ORIENTED_EDGE('',*,*,#9027,.T.);
#11814=ORIENTED_EDGE('',*,*,#8728,.T.);
#11815=ORIENTED_EDGE('',*,*,#9027,.F.);
#11816=ORIENTED_EDGE('',*,*,#8862,.F.);
#11817=ORIENTED_EDGE('',*,*,#9028,.T.);
#11818=ORIENTED_EDGE('',*,*,#8725,.F.);
#11819=ORIENTED_EDGE('',*,*,#9028,.F.);
#11820=ORIENTED_EDGE('',*,*,#8861,.T.);
#11821=ORIENTED_EDGE('',*,*,#8973,.T.);
#11822=ORIENTED_EDGE('',*,*,#8731,.T.);
#11823=ORIENTED_EDGE('',*,*,#8976,.F.);
#11824=ORIENTED_EDGE('',*,*,#8859,.F.);
#11825=ORIENTED_EDGE('',*,*,#9029,.T.);
#11826=ORIENTED_EDGE('',*,*,#8732,.T.);
#11827=ORIENTED_EDGE('',*,*,#9029,.F.);
#11828=ORIENTED_EDGE('',*,*,#8858,.F.);
#11829=ORIENTED_EDGE('',*,*,#9030,.T.);
#11830=ORIENTED_EDGE('',*,*,#8729,.F.);
#11831=ORIENTED_EDGE('',*,*,#9030,.F.);
#11832=ORIENTED_EDGE('',*,*,#8857,.T.);
#11833=ORIENTED_EDGE('',*,*,#8975,.T.);
#11834=ORIENTED_EDGE('',*,*,#8735,.T.);
#11835=ORIENTED_EDGE('',*,*,#8978,.F.);
#11836=ORIENTED_EDGE('',*,*,#8855,.F.);
#11837=ORIENTED_EDGE('',*,*,#9031,.T.);
#11838=ORIENTED_EDGE('',*,*,#8736,.T.);
#11839=ORIENTED_EDGE('',*,*,#9031,.F.);
#11840=ORIENTED_EDGE('',*,*,#8854,.F.);
#11841=ORIENTED_EDGE('',*,*,#9032,.T.);
#11842=ORIENTED_EDGE('',*,*,#8733,.F.);
#11843=ORIENTED_EDGE('',*,*,#9032,.F.);
#11844=ORIENTED_EDGE('',*,*,#8853,.T.);
#11845=ORIENTED_EDGE('',*,*,#8977,.T.);
#11846=ORIENTED_EDGE('',*,*,#8739,.T.);
#11847=ORIENTED_EDGE('',*,*,#8980,.F.);
#11848=ORIENTED_EDGE('',*,*,#8851,.F.);
#11849=ORIENTED_EDGE('',*,*,#9033,.T.);
#11850=ORIENTED_EDGE('',*,*,#8740,.T.);
#11851=ORIENTED_EDGE('',*,*,#9033,.F.);
#11852=ORIENTED_EDGE('',*,*,#8850,.F.);
#11853=ORIENTED_EDGE('',*,*,#9034,.T.);
#11854=ORIENTED_EDGE('',*,*,#8737,.F.);
#11855=ORIENTED_EDGE('',*,*,#9034,.F.);
#11856=ORIENTED_EDGE('',*,*,#8849,.T.);
#11857=ORIENTED_EDGE('',*,*,#8979,.T.);
#11858=ORIENTED_EDGE('',*,*,#8743,.T.);
#11859=ORIENTED_EDGE('',*,*,#8982,.F.);
#11860=ORIENTED_EDGE('',*,*,#8847,.F.);
#11861=ORIENTED_EDGE('',*,*,#9035,.T.);
#11862=ORIENTED_EDGE('',*,*,#8744,.T.);
#11863=ORIENTED_EDGE('',*,*,#9035,.F.);
#11864=ORIENTED_EDGE('',*,*,#8846,.F.);
#11865=ORIENTED_EDGE('',*,*,#9036,.T.);
#11866=ORIENTED_EDGE('',*,*,#8741,.F.);
#11867=ORIENTED_EDGE('',*,*,#9036,.F.);
#11868=ORIENTED_EDGE('',*,*,#8845,.T.);
#11869=ORIENTED_EDGE('',*,*,#8981,.T.);
#11870=ORIENTED_EDGE('',*,*,#8747,.T.);
#11871=ORIENTED_EDGE('',*,*,#8984,.F.);
#11872=ORIENTED_EDGE('',*,*,#8843,.F.);
#11873=ORIENTED_EDGE('',*,*,#9037,.T.);
#11874=ORIENTED_EDGE('',*,*,#8748,.T.);
#11875=ORIENTED_EDGE('',*,*,#9037,.F.);
#11876=ORIENTED_EDGE('',*,*,#8842,.F.);
#11877=ORIENTED_EDGE('',*,*,#9038,.T.);
#11878=ORIENTED_EDGE('',*,*,#8745,.F.);
#11879=ORIENTED_EDGE('',*,*,#9038,.F.);
#11880=ORIENTED_EDGE('',*,*,#8841,.T.);
#11881=ORIENTED_EDGE('',*,*,#8983,.T.);
#11882=ORIENTED_EDGE('',*,*,#8751,.T.);
#11883=ORIENTED_EDGE('',*,*,#8986,.F.);
#11884=ORIENTED_EDGE('',*,*,#8839,.F.);
#11885=ORIENTED_EDGE('',*,*,#9039,.T.);
#11886=ORIENTED_EDGE('',*,*,#8752,.T.);
#11887=ORIENTED_EDGE('',*,*,#9039,.F.);
#11888=ORIENTED_EDGE('',*,*,#8838,.F.);
#11889=ORIENTED_EDGE('',*,*,#9040,.T.);
#11890=ORIENTED_EDGE('',*,*,#8749,.F.);
#11891=ORIENTED_EDGE('',*,*,#9040,.F.);
#11892=ORIENTED_EDGE('',*,*,#8837,.T.);
#11893=ORIENTED_EDGE('',*,*,#8985,.T.);
#11894=ORIENTED_EDGE('',*,*,#8755,.T.);
#11895=ORIENTED_EDGE('',*,*,#8988,.F.);
#11896=ORIENTED_EDGE('',*,*,#8835,.F.);
#11897=ORIENTED_EDGE('',*,*,#9041,.T.);
#11898=ORIENTED_EDGE('',*,*,#8756,.T.);
#11899=ORIENTED_EDGE('',*,*,#9041,.F.);
#11900=ORIENTED_EDGE('',*,*,#8834,.F.);
#11901=ORIENTED_EDGE('',*,*,#9042,.T.);
#11902=ORIENTED_EDGE('',*,*,#8753,.F.);
#11903=ORIENTED_EDGE('',*,*,#9042,.F.);
#11904=ORIENTED_EDGE('',*,*,#8833,.T.);
#11905=ORIENTED_EDGE('',*,*,#8987,.T.);
#11906=ORIENTED_EDGE('',*,*,#8759,.T.);
#11907=ORIENTED_EDGE('',*,*,#8990,.F.);
#11908=ORIENTED_EDGE('',*,*,#8831,.F.);
#11909=ORIENTED_EDGE('',*,*,#9043,.T.);
#11910=ORIENTED_EDGE('',*,*,#8760,.T.);
#11911=ORIENTED_EDGE('',*,*,#9043,.F.);
#11912=ORIENTED_EDGE('',*,*,#8830,.F.);
#11913=ORIENTED_EDGE('',*,*,#9044,.T.);
#11914=ORIENTED_EDGE('',*,*,#8757,.F.);
#11915=ORIENTED_EDGE('',*,*,#9044,.F.);
#11916=ORIENTED_EDGE('',*,*,#8829,.T.);
#11917=ORIENTED_EDGE('',*,*,#8989,.T.);
#11918=ORIENTED_EDGE('',*,*,#8763,.T.);
#11919=ORIENTED_EDGE('',*,*,#8992,.F.);
#11920=ORIENTED_EDGE('',*,*,#8827,.F.);
#11921=ORIENTED_EDGE('',*,*,#9045,.T.);
#11922=ORIENTED_EDGE('',*,*,#8764,.T.);
#11923=ORIENTED_EDGE('',*,*,#9045,.F.);
#11924=ORIENTED_EDGE('',*,*,#8826,.F.);
#11925=ORIENTED_EDGE('',*,*,#9046,.T.);
#11926=ORIENTED_EDGE('',*,*,#8761,.F.);
#11927=ORIENTED_EDGE('',*,*,#9046,.F.);
#11928=ORIENTED_EDGE('',*,*,#8825,.T.);
#11929=ORIENTED_EDGE('',*,*,#8991,.T.);
#11930=ORIENTED_EDGE('',*,*,#8767,.T.);
#11931=ORIENTED_EDGE('',*,*,#8994,.F.);
#11932=ORIENTED_EDGE('',*,*,#8823,.F.);
#11933=ORIENTED_EDGE('',*,*,#9047,.T.);
#11934=ORIENTED_EDGE('',*,*,#8768,.T.);
#11935=ORIENTED_EDGE('',*,*,#9047,.F.);
#11936=ORIENTED_EDGE('',*,*,#8822,.F.);
#11937=ORIENTED_EDGE('',*,*,#9048,.T.);
#11938=ORIENTED_EDGE('',*,*,#8765,.F.);
#11939=ORIENTED_EDGE('',*,*,#9048,.F.);
#11940=ORIENTED_EDGE('',*,*,#8821,.T.);
#11941=ORIENTED_EDGE('',*,*,#8993,.T.);
#11942=ORIENTED_EDGE('',*,*,#8771,.T.);
#11943=ORIENTED_EDGE('',*,*,#8996,.F.);
#11944=ORIENTED_EDGE('',*,*,#8819,.F.);
#11945=ORIENTED_EDGE('',*,*,#9049,.T.);
#11946=ORIENTED_EDGE('',*,*,#8772,.T.);
#11947=ORIENTED_EDGE('',*,*,#9049,.F.);
#11948=ORIENTED_EDGE('',*,*,#8818,.F.);
#11949=ORIENTED_EDGE('',*,*,#9050,.T.);
#11950=ORIENTED_EDGE('',*,*,#8769,.F.);
#11951=ORIENTED_EDGE('',*,*,#9050,.F.);
#11952=ORIENTED_EDGE('',*,*,#8817,.T.);
#11953=ORIENTED_EDGE('',*,*,#8995,.T.);
#11954=ORIENTED_EDGE('',*,*,#8775,.T.);
#11955=ORIENTED_EDGE('',*,*,#8998,.F.);
#11956=ORIENTED_EDGE('',*,*,#8815,.F.);
#11957=ORIENTED_EDGE('',*,*,#9051,.T.);
#11958=ORIENTED_EDGE('',*,*,#8776,.T.);
#11959=ORIENTED_EDGE('',*,*,#9051,.F.);
#11960=ORIENTED_EDGE('',*,*,#8814,.F.);
#11961=ORIENTED_EDGE('',*,*,#9052,.T.);
#11962=ORIENTED_EDGE('',*,*,#8773,.F.);
#11963=ORIENTED_EDGE('',*,*,#9052,.F.);
#11964=ORIENTED_EDGE('',*,*,#8813,.T.);
#11965=ORIENTED_EDGE('',*,*,#8997,.T.);
#11966=ORIENTED_EDGE('',*,*,#8779,.T.);
#11967=ORIENTED_EDGE('',*,*,#9000,.F.);
#11968=ORIENTED_EDGE('',*,*,#8811,.F.);
#11969=ORIENTED_EDGE('',*,*,#9053,.T.);
#11970=ORIENTED_EDGE('',*,*,#8780,.T.);
#11971=ORIENTED_EDGE('',*,*,#9053,.F.);
#11972=ORIENTED_EDGE('',*,*,#8810,.F.);
#11973=ORIENTED_EDGE('',*,*,#9054,.T.);
#11974=ORIENTED_EDGE('',*,*,#8777,.F.);
#11975=ORIENTED_EDGE('',*,*,#9054,.F.);
#11976=ORIENTED_EDGE('',*,*,#8809,.T.);
#11977=ORIENTED_EDGE('',*,*,#8999,.T.);
#11978=ORIENTED_EDGE('',*,*,#8783,.T.);
#11979=ORIENTED_EDGE('',*,*,#9002,.F.);
#11980=ORIENTED_EDGE('',*,*,#8807,.F.);
#11981=ORIENTED_EDGE('',*,*,#9055,.T.);
#11982=ORIENTED_EDGE('',*,*,#8784,.T.);
#11983=ORIENTED_EDGE('',*,*,#9055,.F.);
#11984=ORIENTED_EDGE('',*,*,#8806,.F.);
#11985=ORIENTED_EDGE('',*,*,#9056,.T.);
#11986=ORIENTED_EDGE('',*,*,#8781,.F.);
#11987=ORIENTED_EDGE('',*,*,#9056,.F.);
#11988=ORIENTED_EDGE('',*,*,#8805,.T.);
#11989=ORIENTED_EDGE('',*,*,#9001,.T.);
#11990=ORIENTED_EDGE('',*,*,#8787,.T.);
#11991=ORIENTED_EDGE('',*,*,#9004,.F.);
#11992=ORIENTED_EDGE('',*,*,#8803,.F.);
#11993=ORIENTED_EDGE('',*,*,#9057,.T.);
#11994=ORIENTED_EDGE('',*,*,#8788,.T.);
#11995=ORIENTED_EDGE('',*,*,#9057,.F.);
#11996=ORIENTED_EDGE('',*,*,#8802,.F.);
#11997=ORIENTED_EDGE('',*,*,#9058,.T.);
#11998=ORIENTED_EDGE('',*,*,#8785,.F.);
#11999=ORIENTED_EDGE('',*,*,#9058,.F.);
#12000=ORIENTED_EDGE('',*,*,#8801,.T.);
#12001=ORIENTED_EDGE('',*,*,#9003,.T.);
#12002=ORIENTED_EDGE('',*,*,#8791,.T.);
#12003=ORIENTED_EDGE('',*,*,#8928,.F.);
#12004=ORIENTED_EDGE('',*,*,#8799,.F.);
#12005=ORIENTED_EDGE('',*,*,#9059,.T.);
#12006=ORIENTED_EDGE('',*,*,#8792,.T.);
#12007=ORIENTED_EDGE('',*,*,#9059,.F.);
#12008=ORIENTED_EDGE('',*,*,#8798,.F.);
#12009=ORIENTED_EDGE('',*,*,#9060,.T.);
#12010=ORIENTED_EDGE('',*,*,#8789,.F.);
#12011=ORIENTED_EDGE('',*,*,#9060,.F.);
#12012=ORIENTED_EDGE('',*,*,#8797,.T.);
#12013=ORIENTED_EDGE('',*,*,#8927,.T.);
#12014=ORIENTED_EDGE('',*,*,#9005,.T.);
#12015=ORIENTED_EDGE('',*,*,#8659,.T.);
#12016=ORIENTED_EDGE('',*,*,#9008,.F.);
#12017=ORIENTED_EDGE('',*,*,#8793,.T.);
#12018=ORIENTED_EDGE('',*,*,#9061,.T.);
#12019=ORIENTED_EDGE('',*,*,#9062,.F.);
#12020=ORIENTED_EDGE('',*,*,#9063,.F.);
#12021=ORIENTED_EDGE('',*,*,#9064,.F.);
#12022=ORIENTED_EDGE('',*,*,#9065,.T.);
#12023=ORIENTED_EDGE('',*,*,#9066,.F.);
#12024=ORIENTED_EDGE('',*,*,#9064,.T.);
#12025=ORIENTED_EDGE('',*,*,#9067,.F.);
#12026=ORIENTED_EDGE('',*,*,#9065,.F.);
#12027=ORIENTED_EDGE('',*,*,#9068,.F.);
#12028=ORIENTED_EDGE('',*,*,#9062,.T.);
#12029=ORIENTED_EDGE('',*,*,#9061,.F.);
#12030=ORIENTED_EDGE('',*,*,#9069,.T.);
#12031=ORIENTED_EDGE('',*,*,#9070,.F.);
#12032=ORIENTED_EDGE('',*,*,#9071,.F.);
#12033=ORIENTED_EDGE('',*,*,#9072,.F.);
#12034=ORIENTED_EDGE('',*,*,#9073,.T.);
#12035=ORIENTED_EDGE('',*,*,#9074,.F.);
#12036=ORIENTED_EDGE('',*,*,#9072,.T.);
#12037=ORIENTED_EDGE('',*,*,#9075,.F.);
#12038=ORIENTED_EDGE('',*,*,#9073,.F.);
#12039=ORIENTED_EDGE('',*,*,#9076,.F.);
#12040=ORIENTED_EDGE('',*,*,#9070,.T.);
#12041=ORIENTED_EDGE('',*,*,#9069,.F.);
#12042=ORIENTED_EDGE('',*,*,#9077,.T.);
#12043=ORIENTED_EDGE('',*,*,#9078,.F.);
#12044=ORIENTED_EDGE('',*,*,#9079,.F.);
#12045=ORIENTED_EDGE('',*,*,#9080,.F.);
#12046=ORIENTED_EDGE('',*,*,#9081,.T.);
#12047=ORIENTED_EDGE('',*,*,#9082,.F.);
#12048=ORIENTED_EDGE('',*,*,#9080,.T.);
#12049=ORIENTED_EDGE('',*,*,#9083,.F.);
#12050=ORIENTED_EDGE('',*,*,#9081,.F.);
#12051=ORIENTED_EDGE('',*,*,#9084,.F.);
#12052=ORIENTED_EDGE('',*,*,#9078,.T.);
#12053=ORIENTED_EDGE('',*,*,#9077,.F.);
#12054=ORIENTED_EDGE('',*,*,#9085,.F.);
#12055=ORIENTED_EDGE('',*,*,#9086,.F.);
#12056=ORIENTED_EDGE('',*,*,#9087,.T.);
#12057=ORIENTED_EDGE('',*,*,#9088,.F.);
#12058=ORIENTED_EDGE('',*,*,#9089,.T.);
#12059=ORIENTED_EDGE('',*,*,#9090,.F.);
#12060=ORIENTED_EDGE('',*,*,#9091,.F.);
#12061=ORIENTED_EDGE('',*,*,#9087,.F.);
#12062=ORIENTED_EDGE('',*,*,#9092,.F.);
#12063=ORIENTED_EDGE('',*,*,#9093,.T.);
#12064=ORIENTED_EDGE('',*,*,#9089,.F.);
#12065=ORIENTED_EDGE('',*,*,#9094,.T.);
#12066=ORIENTED_EDGE('',*,*,#9095,.F.);
#12067=ORIENTED_EDGE('',*,*,#9096,.T.);
#12068=ORIENTED_EDGE('',*,*,#9097,.F.);
#12069=ORIENTED_EDGE('',*,*,#9093,.F.);
#12070=ORIENTED_EDGE('',*,*,#9098,.F.);
#12071=ORIENTED_EDGE('',*,*,#9099,.F.);
#12072=ORIENTED_EDGE('',*,*,#9100,.F.);
#12073=ORIENTED_EDGE('',*,*,#9101,.T.);
#12074=ORIENTED_EDGE('',*,*,#9094,.F.);
#12075=ORIENTED_EDGE('',*,*,#9102,.T.);
#12076=ORIENTED_EDGE('',*,*,#9103,.F.);
#12077=ORIENTED_EDGE('',*,*,#9104,.F.);
#12078=ORIENTED_EDGE('',*,*,#9101,.F.);
#12079=ORIENTED_EDGE('',*,*,#9105,.F.);
#12080=ORIENTED_EDGE('',*,*,#9106,.T.);
#12081=ORIENTED_EDGE('',*,*,#9107,.F.);
#12082=ORIENTED_EDGE('',*,*,#9108,.F.);
#12083=ORIENTED_EDGE('',*,*,#9102,.F.);
#12084=ORIENTED_EDGE('',*,*,#9109,.F.);
#12085=ORIENTED_EDGE('',*,*,#9110,.F.);
#12086=ORIENTED_EDGE('',*,*,#9106,.F.);
#12087=ORIENTED_EDGE('',*,*,#9111,.F.);
#12088=ORIENTED_EDGE('',*,*,#9112,.F.);
#12089=ORIENTED_EDGE('',*,*,#9113,.T.);
#12090=ORIENTED_EDGE('',*,*,#9114,.F.);
#12091=ORIENTED_EDGE('',*,*,#9115,.T.);
#12092=ORIENTED_EDGE('',*,*,#9116,.T.);
#12093=ORIENTED_EDGE('',*,*,#9117,.F.);
#12094=ORIENTED_EDGE('',*,*,#9118,.T.);
#12095=ORIENTED_EDGE('',*,*,#9117,.T.);
#12096=ORIENTED_EDGE('',*,*,#9119,.T.);
#12097=ORIENTED_EDGE('',*,*,#9120,.F.);
#12098=ORIENTED_EDGE('',*,*,#9121,.T.);
#12099=ORIENTED_EDGE('',*,*,#9120,.T.);
#12100=ORIENTED_EDGE('',*,*,#9122,.T.);
#12101=ORIENTED_EDGE('',*,*,#9123,.F.);
#12102=ORIENTED_EDGE('',*,*,#9124,.T.);
#12103=ORIENTED_EDGE('',*,*,#9123,.T.);
#12104=ORIENTED_EDGE('',*,*,#9125,.T.);
#12105=ORIENTED_EDGE('',*,*,#9126,.F.);
#12106=ORIENTED_EDGE('',*,*,#9127,.T.);
#12107=ORIENTED_EDGE('',*,*,#9126,.T.);
#12108=ORIENTED_EDGE('',*,*,#9128,.T.);
#12109=ORIENTED_EDGE('',*,*,#9129,.F.);
#12110=ORIENTED_EDGE('',*,*,#9130,.F.);
#12111=ORIENTED_EDGE('',*,*,#9129,.T.);
#12112=ORIENTED_EDGE('',*,*,#9131,.T.);
#12113=ORIENTED_EDGE('',*,*,#9115,.F.);
#12114=ORIENTED_EDGE('',*,*,#9132,.F.);
#12115=ORIENTED_EDGE('',*,*,#9133,.F.);
#12116=ORIENTED_EDGE('',*,*,#9134,.F.);
#12117=ORIENTED_EDGE('',*,*,#9135,.F.);
#12118=ORIENTED_EDGE('',*,*,#9136,.F.);
#12119=ORIENTED_EDGE('',*,*,#9137,.F.);
#12120=ORIENTED_EDGE('',*,*,#9130,.T.);
#12121=ORIENTED_EDGE('',*,*,#9132,.T.);
#12122=ORIENTED_EDGE('',*,*,#9114,.T.);
#12123=ORIENTED_EDGE('',*,*,#9138,.F.);
#12124=ORIENTED_EDGE('',*,*,#9139,.F.);
#12125=ORIENTED_EDGE('',*,*,#9140,.F.);
#12126=ORIENTED_EDGE('',*,*,#9141,.F.);
#12127=ORIENTED_EDGE('',*,*,#9142,.F.);
#12128=ORIENTED_EDGE('',*,*,#9067,.T.);
#12129=ORIENTED_EDGE('',*,*,#9143,.T.);
#12130=ORIENTED_EDGE('',*,*,#9133,.T.);
#12131=ORIENTED_EDGE('',*,*,#9144,.F.);
#12132=ORIENTED_EDGE('',*,*,#9145,.F.);
#12133=ORIENTED_EDGE('',*,*,#9146,.F.);
#12134=ORIENTED_EDGE('',*,*,#9139,.T.);
#12135=ORIENTED_EDGE('',*,*,#9143,.F.);
#12136=ORIENTED_EDGE('',*,*,#9063,.T.);
#12137=ORIENTED_EDGE('',*,*,#9147,.T.);
#12138=ORIENTED_EDGE('',*,*,#9134,.T.);
#12139=ORIENTED_EDGE('',*,*,#9128,.F.);
#12140=ORIENTED_EDGE('',*,*,#9125,.F.);
#12141=ORIENTED_EDGE('',*,*,#9122,.F.);
#12142=ORIENTED_EDGE('',*,*,#9119,.F.);
#12143=ORIENTED_EDGE('',*,*,#9116,.F.);
#12144=ORIENTED_EDGE('',*,*,#9131,.F.);
#12145=ORIENTED_EDGE('',*,*,#9147,.F.);
#12146=ORIENTED_EDGE('',*,*,#9068,.T.);
#12147=ORIENTED_EDGE('',*,*,#9148,.T.);
#12148=ORIENTED_EDGE('',*,*,#9141,.T.);
#12149=ORIENTED_EDGE('',*,*,#9149,.F.);
#12150=ORIENTED_EDGE('',*,*,#9150,.F.);
#12151=ORIENTED_EDGE('',*,*,#9151,.F.);
#12152=ORIENTED_EDGE('',*,*,#9135,.T.);
#12153=ORIENTED_EDGE('',*,*,#9148,.F.);
#12154=ORIENTED_EDGE('',*,*,#9066,.T.);
#12155=ORIENTED_EDGE('',*,*,#9142,.T.);
#12156=ORIENTED_EDGE('',*,*,#9138,.T.);
#12157=ORIENTED_EDGE('',*,*,#9113,.F.);
#12158=ORIENTED_EDGE('',*,*,#9118,.F.);
#12159=ORIENTED_EDGE('',*,*,#9121,.F.);
#12160=ORIENTED_EDGE('',*,*,#9124,.F.);
#12161=ORIENTED_EDGE('',*,*,#9127,.F.);
#12162=ORIENTED_EDGE('',*,*,#9137,.T.);
#12163=ORIENTED_EDGE('',*,*,#9152,.F.);
#12164=ORIENTED_EDGE('',*,*,#9153,.F.);
#12165=ORIENTED_EDGE('',*,*,#9154,.F.);
#12166=ORIENTED_EDGE('',*,*,#9155,.F.);
#12167=ORIENTED_EDGE('',*,*,#9156,.F.);
#12168=ORIENTED_EDGE('',*,*,#9157,.F.);
#12169=ORIENTED_EDGE('',*,*,#9158,.F.);
#12170=ORIENTED_EDGE('',*,*,#9159,.F.);
#12171=ORIENTED_EDGE('',*,*,#9160,.F.);
#12172=ORIENTED_EDGE('',*,*,#9161,.F.);
#12173=ORIENTED_EDGE('',*,*,#9162,.F.);
#12174=ORIENTED_EDGE('',*,*,#9163,.F.);
#12175=ORIENTED_EDGE('',*,*,#9164,.F.);
#12176=ORIENTED_EDGE('',*,*,#9165,.F.);
#12177=ORIENTED_EDGE('',*,*,#9166,.F.);
#12178=ORIENTED_EDGE('',*,*,#9167,.F.);
#12179=ORIENTED_EDGE('',*,*,#9168,.T.);
#12180=ORIENTED_EDGE('',*,*,#9169,.T.);
#12181=ORIENTED_EDGE('',*,*,#9170,.T.);
#12182=ORIENTED_EDGE('',*,*,#9171,.F.);
#12183=ORIENTED_EDGE('',*,*,#9172,.T.);
#12184=ORIENTED_EDGE('',*,*,#9171,.T.);
#12185=ORIENTED_EDGE('',*,*,#9173,.T.);
#12186=ORIENTED_EDGE('',*,*,#9174,.F.);
#12187=ORIENTED_EDGE('',*,*,#9175,.T.);
#12188=ORIENTED_EDGE('',*,*,#9174,.T.);
#12189=ORIENTED_EDGE('',*,*,#9176,.T.);
#12190=ORIENTED_EDGE('',*,*,#9177,.F.);
#12191=ORIENTED_EDGE('',*,*,#9178,.T.);
#12192=ORIENTED_EDGE('',*,*,#9177,.T.);
#12193=ORIENTED_EDGE('',*,*,#9179,.T.);
#12194=ORIENTED_EDGE('',*,*,#9180,.F.);
#12195=ORIENTED_EDGE('',*,*,#9181,.T.);
#12196=ORIENTED_EDGE('',*,*,#9180,.T.);
#12197=ORIENTED_EDGE('',*,*,#9182,.T.);
#12198=ORIENTED_EDGE('',*,*,#9183,.F.);
#12199=ORIENTED_EDGE('',*,*,#9184,.T.);
#12200=ORIENTED_EDGE('',*,*,#9183,.T.);
#12201=ORIENTED_EDGE('',*,*,#9185,.T.);
#12202=ORIENTED_EDGE('',*,*,#9186,.F.);
#12203=ORIENTED_EDGE('',*,*,#9187,.T.);
#12204=ORIENTED_EDGE('',*,*,#9186,.T.);
#12205=ORIENTED_EDGE('',*,*,#9188,.T.);
#12206=ORIENTED_EDGE('',*,*,#9189,.F.);
#12207=ORIENTED_EDGE('',*,*,#9190,.T.);
#12208=ORIENTED_EDGE('',*,*,#9191,.T.);
#12209=ORIENTED_EDGE('',*,*,#9192,.T.);
#12210=ORIENTED_EDGE('',*,*,#9193,.F.);
#12211=ORIENTED_EDGE('',*,*,#9194,.T.);
#12212=ORIENTED_EDGE('',*,*,#9195,.T.);
#12213=ORIENTED_EDGE('',*,*,#9196,.T.);
#12214=ORIENTED_EDGE('',*,*,#9197,.F.);
#12215=ORIENTED_EDGE('',*,*,#9198,.T.);
#12216=ORIENTED_EDGE('',*,*,#9197,.T.);
#12217=ORIENTED_EDGE('',*,*,#9199,.T.);
#12218=ORIENTED_EDGE('',*,*,#9160,.T.);
#12219=ORIENTED_EDGE('',*,*,#9200,.F.);
#12220=ORIENTED_EDGE('',*,*,#9201,.T.);
#12221=ORIENTED_EDGE('',*,*,#9202,.T.);
#12222=ORIENTED_EDGE('',*,*,#9203,.T.);
#12223=ORIENTED_EDGE('',*,*,#9195,.F.);
#12224=ORIENTED_EDGE('',*,*,#9204,.F.);
#12225=ORIENTED_EDGE('',*,*,#9074,.T.);
#12226=ORIENTED_EDGE('',*,*,#9205,.T.);
#12227=ORIENTED_EDGE('',*,*,#9167,.T.);
#12228=ORIENTED_EDGE('',*,*,#9206,.F.);
#12229=ORIENTED_EDGE('',*,*,#9071,.T.);
#12230=ORIENTED_EDGE('',*,*,#9207,.T.);
#12231=ORIENTED_EDGE('',*,*,#9157,.T.);
#12232=ORIENTED_EDGE('',*,*,#9207,.F.);
#12233=ORIENTED_EDGE('',*,*,#9076,.T.);
#12234=ORIENTED_EDGE('',*,*,#9204,.T.);
#12235=ORIENTED_EDGE('',*,*,#9166,.T.);
#12236=ORIENTED_EDGE('',*,*,#9208,.F.);
#12237=ORIENTED_EDGE('',*,*,#9209,.T.);
#12238=ORIENTED_EDGE('',*,*,#9210,.F.);
#12239=ORIENTED_EDGE('',*,*,#9158,.T.);
#12240=ORIENTED_EDGE('',*,*,#9211,.F.);
#12241=ORIENTED_EDGE('',*,*,#9083,.T.);
#12242=ORIENTED_EDGE('',*,*,#9212,.T.);
#12243=ORIENTED_EDGE('',*,*,#9152,.T.);
#12244=ORIENTED_EDGE('',*,*,#9213,.F.);
#12245=ORIENTED_EDGE('',*,*,#9212,.F.);
#12246=ORIENTED_EDGE('',*,*,#9079,.T.);
#12247=ORIENTED_EDGE('',*,*,#9214,.T.);
#12248=ORIENTED_EDGE('',*,*,#9153,.T.);
#12249=ORIENTED_EDGE('',*,*,#9214,.F.);
#12250=ORIENTED_EDGE('',*,*,#9084,.T.);
#12251=ORIENTED_EDGE('',*,*,#9215,.T.);
#12252=ORIENTED_EDGE('',*,*,#9216,.F.);
#12253=ORIENTED_EDGE('',*,*,#9154,.T.);
#12254=ORIENTED_EDGE('',*,*,#9215,.F.);
#12255=ORIENTED_EDGE('',*,*,#9082,.T.);
#12256=ORIENTED_EDGE('',*,*,#9211,.T.);
#12257=ORIENTED_EDGE('',*,*,#9217,.T.);
#12258=ORIENTED_EDGE('',*,*,#9200,.T.);
#12259=ORIENTED_EDGE('',*,*,#9163,.T.);
#12260=ORIENTED_EDGE('',*,*,#9218,.F.);
#12261=ORIENTED_EDGE('',*,*,#9219,.F.);
#12262=ORIENTED_EDGE('',*,*,#9220,.F.);
#12263=ORIENTED_EDGE('',*,*,#9221,.F.);
#12264=ORIENTED_EDGE('',*,*,#9222,.F.);
#12265=ORIENTED_EDGE('',*,*,#9223,.F.);
#12266=ORIENTED_EDGE('',*,*,#9224,.F.);
#12267=ORIENTED_EDGE('',*,*,#9225,.F.);
#12268=ORIENTED_EDGE('',*,*,#9226,.F.);
#12269=ORIENTED_EDGE('',*,*,#9227,.F.);
#12270=ORIENTED_EDGE('',*,*,#9228,.F.);
#12271=ORIENTED_EDGE('',*,*,#9229,.F.);
#12272=ORIENTED_EDGE('',*,*,#9230,.F.);
#12273=ORIENTED_EDGE('',*,*,#9231,.F.);
#12274=ORIENTED_EDGE('',*,*,#9232,.F.);
#12275=ORIENTED_EDGE('',*,*,#9233,.F.);
#12276=ORIENTED_EDGE('',*,*,#9234,.F.);
#12277=ORIENTED_EDGE('',*,*,#9235,.F.);
#12278=ORIENTED_EDGE('',*,*,#9236,.F.);
#12279=ORIENTED_EDGE('',*,*,#9086,.T.);
#12280=ORIENTED_EDGE('',*,*,#9237,.F.);
#12281=ORIENTED_EDGE('',*,*,#9109,.T.);
#12282=ORIENTED_EDGE('',*,*,#9238,.F.);
#12283=ORIENTED_EDGE('',*,*,#9239,.F.);
#12284=ORIENTED_EDGE('',*,*,#9240,.T.);
#12285=ORIENTED_EDGE('',*,*,#9229,.T.);
#12286=ORIENTED_EDGE('',*,*,#9241,.F.);
#12287=ORIENTED_EDGE('',*,*,#9227,.T.);
#12288=ORIENTED_EDGE('',*,*,#9099,.T.);
#12289=ORIENTED_EDGE('',*,*,#9233,.T.);
#12290=ORIENTED_EDGE('',*,*,#9096,.F.);
#12291=ORIENTED_EDGE('',*,*,#9231,.T.);
#12292=ORIENTED_EDGE('',*,*,#9242,.F.);
#12293=ORIENTED_EDGE('',*,*,#9235,.T.);
#12294=ORIENTED_EDGE('',*,*,#9243,.T.);
#12295=ORIENTED_EDGE('',*,*,#9221,.T.);
#12296=ORIENTED_EDGE('',*,*,#9095,.T.);
#12297=ORIENTED_EDGE('',*,*,#9104,.T.);
#12298=ORIENTED_EDGE('',*,*,#9244,.T.);
#12299=ORIENTED_EDGE('',*,*,#9224,.T.);
#12300=ORIENTED_EDGE('',*,*,#9241,.T.);
#12301=ORIENTED_EDGE('',*,*,#9228,.T.);
#12302=ORIENTED_EDGE('',*,*,#9098,.T.);
#12303=ORIENTED_EDGE('',*,*,#9092,.T.);
#12304=ORIENTED_EDGE('',*,*,#9236,.T.);
#12305=ORIENTED_EDGE('',*,*,#9222,.T.);
#12306=ORIENTED_EDGE('',*,*,#9243,.F.);
#12307=ORIENTED_EDGE('',*,*,#9234,.T.);
#12308=ORIENTED_EDGE('',*,*,#9245,.T.);
#12309=ORIENTED_EDGE('',*,*,#9108,.T.);
#12310=ORIENTED_EDGE('',*,*,#9246,.T.);
#12311=ORIENTED_EDGE('',*,*,#9247,.T.);
#12312=ORIENTED_EDGE('',*,*,#9088,.T.);
#12313=ORIENTED_EDGE('',*,*,#9248,.T.);
#12314=ORIENTED_EDGE('',*,*,#9249,.T.);
#12315=ORIENTED_EDGE('',*,*,#9250,.T.);
#12316=ORIENTED_EDGE('',*,*,#9251,.T.);
#12317=ORIENTED_EDGE('',*,*,#9252,.F.);
#12318=ORIENTED_EDGE('',*,*,#9253,.T.);
#12319=ORIENTED_EDGE('',*,*,#9254,.T.);
#12320=ORIENTED_EDGE('',*,*,#9191,.F.);
#12321=ORIENTED_EDGE('',*,*,#9255,.T.);
#12322=ORIENTED_EDGE('',*,*,#9256,.T.);
#12323=ORIENTED_EDGE('',*,*,#9252,.T.);
#12324=ORIENTED_EDGE('',*,*,#9257,.T.);
#12325=ORIENTED_EDGE('',*,*,#9112,.T.);
#12326=ORIENTED_EDGE('',*,*,#9258,.T.);
#12327=ORIENTED_EDGE('',*,*,#9193,.T.);
#12328=ORIENTED_EDGE('',*,*,#9259,.T.);
#12329=ORIENTED_EDGE('',*,*,#9260,.T.);
#12330=ORIENTED_EDGE('',*,*,#9250,.F.);
#12331=ORIENTED_EDGE('',*,*,#9261,.T.);
#12332=ORIENTED_EDGE('',*,*,#9262,.T.);
#12333=ORIENTED_EDGE('',*,*,#9263,.T.);
#12334=ORIENTED_EDGE('',*,*,#9264,.F.);
#12335=ORIENTED_EDGE('',*,*,#9265,.T.);
#12336=ORIENTED_EDGE('',*,*,#9266,.T.);
#12337=ORIENTED_EDGE('',*,*,#9169,.F.);
#12338=ORIENTED_EDGE('',*,*,#9267,.T.);
#12339=ORIENTED_EDGE('',*,*,#9268,.T.);
#12340=ORIENTED_EDGE('',*,*,#9264,.T.);
#12341=ORIENTED_EDGE('',*,*,#9269,.F.);
#12342=ORIENTED_EDGE('',*,*,#9150,.T.);
#12343=ORIENTED_EDGE('',*,*,#9270,.T.);
#12344=ORIENTED_EDGE('',*,*,#9271,.T.);
#12345=ORIENTED_EDGE('',*,*,#9262,.F.);
#12346=ORIENTED_EDGE('',*,*,#9272,.T.);
#12347=ORIENTED_EDGE('',*,*,#9273,.T.);
#12348=ORIENTED_EDGE('',*,*,#9274,.T.);
#12349=ORIENTED_EDGE('',*,*,#9275,.F.);
#12350=ORIENTED_EDGE('',*,*,#9276,.F.);
#12351=ORIENTED_EDGE('',*,*,#9277,.T.);
#12352=ORIENTED_EDGE('',*,*,#9278,.T.);
#12353=ORIENTED_EDGE('',*,*,#9273,.F.);
#12354=ORIENTED_EDGE('',*,*,#9279,.F.);
#12355=ORIENTED_EDGE('',*,*,#9280,.T.);
#12356=ORIENTED_EDGE('',*,*,#9281,.T.);
#12357=ORIENTED_EDGE('',*,*,#9277,.F.);
#12358=ORIENTED_EDGE('',*,*,#9282,.F.);
#12359=ORIENTED_EDGE('',*,*,#9275,.T.);
#12360=ORIENTED_EDGE('',*,*,#9283,.T.);
#12361=ORIENTED_EDGE('',*,*,#9280,.F.);
#12362=ORIENTED_EDGE('',*,*,#9284,.F.);
#12363=ORIENTED_EDGE('',*,*,#9285,.T.);
#12364=ORIENTED_EDGE('',*,*,#9286,.T.);
#12365=ORIENTED_EDGE('',*,*,#9287,.F.);
#12366=ORIENTED_EDGE('',*,*,#9288,.F.);
#12367=ORIENTED_EDGE('',*,*,#9289,.T.);
#12368=ORIENTED_EDGE('',*,*,#9290,.T.);
#12369=ORIENTED_EDGE('',*,*,#9285,.F.);
#12370=ORIENTED_EDGE('',*,*,#9291,.F.);
#12371=ORIENTED_EDGE('',*,*,#9292,.T.);
#12372=ORIENTED_EDGE('',*,*,#9293,.T.);
#12373=ORIENTED_EDGE('',*,*,#9289,.F.);
#12374=ORIENTED_EDGE('',*,*,#9294,.F.);
#12375=ORIENTED_EDGE('',*,*,#9287,.T.);
#12376=ORIENTED_EDGE('',*,*,#9295,.T.);
#12377=ORIENTED_EDGE('',*,*,#9292,.F.);
#12378=ORIENTED_EDGE('',*,*,#9296,.F.);
#12379=ORIENTED_EDGE('',*,*,#9297,.T.);
#12380=ORIENTED_EDGE('',*,*,#9298,.T.);
#12381=ORIENTED_EDGE('',*,*,#9299,.F.);
#12382=ORIENTED_EDGE('',*,*,#9300,.F.);
#12383=ORIENTED_EDGE('',*,*,#9301,.F.);
#12384=ORIENTED_EDGE('',*,*,#9218,.T.);
#12385=ORIENTED_EDGE('',*,*,#9162,.T.);
#12386=ORIENTED_EDGE('',*,*,#9302,.T.);
#12387=ORIENTED_EDGE('',*,*,#9301,.T.);
#12388=ORIENTED_EDGE('',*,*,#9303,.T.);
#12389=ORIENTED_EDGE('',*,*,#9304,.T.);
#12390=ORIENTED_EDGE('',*,*,#9305,.F.);
#12391=ORIENTED_EDGE('',*,*,#9304,.F.);
#12392=ORIENTED_EDGE('',*,*,#9306,.T.);
#12393=ORIENTED_EDGE('',*,*,#9300,.T.);
#12394=ORIENTED_EDGE('',*,*,#9307,.F.);
#12395=ORIENTED_EDGE('',*,*,#9308,.T.);
#12396=ORIENTED_EDGE('',*,*,#9309,.T.);
#12397=ORIENTED_EDGE('',*,*,#9296,.T.);
#12398=ORIENTED_EDGE('',*,*,#9294,.T.);
#12399=ORIENTED_EDGE('',*,*,#9291,.T.);
#12400=ORIENTED_EDGE('',*,*,#9288,.T.);
#12401=ORIENTED_EDGE('',*,*,#9284,.T.);
#12402=ORIENTED_EDGE('',*,*,#9282,.T.);
#12403=ORIENTED_EDGE('',*,*,#9279,.T.);
#12404=ORIENTED_EDGE('',*,*,#9276,.T.);
#12405=ORIENTED_EDGE('',*,*,#9257,.F.);
#12406=ORIENTED_EDGE('',*,*,#9249,.F.);
#12407=ORIENTED_EDGE('',*,*,#9256,.F.);
#12408=ORIENTED_EDGE('',*,*,#9310,.T.);
#12409=ORIENTED_EDGE('',*,*,#9272,.F.);
#12410=ORIENTED_EDGE('',*,*,#9261,.F.);
#12411=ORIENTED_EDGE('',*,*,#9268,.F.);
#12412=ORIENTED_EDGE('',*,*,#9311,.T.);
#12413=ORIENTED_EDGE('',*,*,#9306,.F.);
#12414=ORIENTED_EDGE('',*,*,#9303,.F.);
#12415=ORIENTED_EDGE('',*,*,#9309,.F.);
#12416=ORIENTED_EDGE('',*,*,#9312,.T.);
#12417=ORIENTED_EDGE('',*,*,#9110,.T.);
#12418=ORIENTED_EDGE('',*,*,#9258,.F.);
#12419=ORIENTED_EDGE('',*,*,#9111,.T.);
#12420=ORIENTED_EDGE('',*,*,#9237,.T.);
#12421=ORIENTED_EDGE('',*,*,#9313,.T.);
#12422=ORIENTED_EDGE('',*,*,#9314,.T.);
#12423=ORIENTED_EDGE('',*,*,#9159,.T.);
#12424=ORIENTED_EDGE('',*,*,#9210,.T.);
#12425=ORIENTED_EDGE('',*,*,#9315,.F.);
#12426=ORIENTED_EDGE('',*,*,#9201,.F.);
#12427=ORIENTED_EDGE('',*,*,#9194,.F.);
#12428=ORIENTED_EDGE('',*,*,#9198,.F.);
#12429=ORIENTED_EDGE('',*,*,#9217,.F.);
#12430=ORIENTED_EDGE('',*,*,#9213,.T.);
#12431=ORIENTED_EDGE('',*,*,#9155,.T.);
#12432=ORIENTED_EDGE('',*,*,#9216,.T.);
#12433=ORIENTED_EDGE('',*,*,#9219,.T.);
#12434=ORIENTED_EDGE('',*,*,#9305,.T.);
#12435=ORIENTED_EDGE('',*,*,#9311,.F.);
#12436=ORIENTED_EDGE('',*,*,#9267,.F.);
#12437=ORIENTED_EDGE('',*,*,#9168,.F.);
#12438=ORIENTED_EDGE('',*,*,#9172,.F.);
#12439=ORIENTED_EDGE('',*,*,#9175,.F.);
#12440=ORIENTED_EDGE('',*,*,#9178,.F.);
#12441=ORIENTED_EDGE('',*,*,#9181,.F.);
#12442=ORIENTED_EDGE('',*,*,#9184,.F.);
#12443=ORIENTED_EDGE('',*,*,#9187,.F.);
#12444=ORIENTED_EDGE('',*,*,#9316,.F.);
#12445=ORIENTED_EDGE('',*,*,#9144,.T.);
#12446=ORIENTED_EDGE('',*,*,#9136,.T.);
#12447=ORIENTED_EDGE('',*,*,#9151,.T.);
#12448=ORIENTED_EDGE('',*,*,#9269,.T.);
#12449=ORIENTED_EDGE('',*,*,#9310,.F.);
#12450=ORIENTED_EDGE('',*,*,#9255,.F.);
#12451=ORIENTED_EDGE('',*,*,#9190,.F.);
#12452=ORIENTED_EDGE('',*,*,#9205,.F.);
#12453=ORIENTED_EDGE('',*,*,#9075,.T.);
#12454=ORIENTED_EDGE('',*,*,#9206,.T.);
#12455=ORIENTED_EDGE('',*,*,#9156,.T.);
#12456=ORIENTED_EDGE('',*,*,#9314,.F.);
#12457=ORIENTED_EDGE('',*,*,#9317,.T.);
#12458=ORIENTED_EDGE('',*,*,#9318,.T.);
#12459=ORIENTED_EDGE('',*,*,#9164,.T.);
#12460=ORIENTED_EDGE('',*,*,#9270,.F.);
#12461=ORIENTED_EDGE('',*,*,#9149,.T.);
#12462=ORIENTED_EDGE('',*,*,#9140,.T.);
#12463=ORIENTED_EDGE('',*,*,#9146,.T.);
#12464=ORIENTED_EDGE('',*,*,#9319,.F.);
#12465=ORIENTED_EDGE('',*,*,#9188,.F.);
#12466=ORIENTED_EDGE('',*,*,#9185,.F.);
#12467=ORIENTED_EDGE('',*,*,#9182,.F.);
#12468=ORIENTED_EDGE('',*,*,#9179,.F.);
#12469=ORIENTED_EDGE('',*,*,#9176,.F.);
#12470=ORIENTED_EDGE('',*,*,#9173,.F.);
#12471=ORIENTED_EDGE('',*,*,#9170,.F.);
#12472=ORIENTED_EDGE('',*,*,#9266,.F.);
#12473=ORIENTED_EDGE('',*,*,#9320,.T.);
#12474=ORIENTED_EDGE('',*,*,#9302,.F.);
#12475=ORIENTED_EDGE('',*,*,#9161,.T.);
#12476=ORIENTED_EDGE('',*,*,#9199,.F.);
#12477=ORIENTED_EDGE('',*,*,#9196,.F.);
#12478=ORIENTED_EDGE('',*,*,#9203,.F.);
#12479=ORIENTED_EDGE('',*,*,#9321,.F.);
#12480=ORIENTED_EDGE('',*,*,#9208,.T.);
#12481=ORIENTED_EDGE('',*,*,#9165,.T.);
#12482=ORIENTED_EDGE('',*,*,#9318,.F.);
#12483=ORIENTED_EDGE('',*,*,#9322,.T.);
#12484=ORIENTED_EDGE('',*,*,#9248,.F.);
#12485=ORIENTED_EDGE('',*,*,#9091,.T.);
#12486=ORIENTED_EDGE('',*,*,#9323,.F.);
#12487=ORIENTED_EDGE('',*,*,#9223,.T.);
#12488=ORIENTED_EDGE('',*,*,#9239,.T.);
#12489=ORIENTED_EDGE('',*,*,#9225,.T.);
#12490=ORIENTED_EDGE('',*,*,#9244,.F.);
#12491=ORIENTED_EDGE('',*,*,#9103,.T.);
#12492=ORIENTED_EDGE('',*,*,#9245,.F.);
#12493=ORIENTED_EDGE('',*,*,#9324,.T.);
#12494=ORIENTED_EDGE('',*,*,#9259,.F.);
#12495=ORIENTED_EDGE('',*,*,#9192,.F.);
#12496=ORIENTED_EDGE('',*,*,#9254,.F.);
#12497=ORIENTED_EDGE('',*,*,#9325,.T.);
#12498=ORIENTED_EDGE('',*,*,#9265,.F.);
#12499=ORIENTED_EDGE('',*,*,#9326,.T.);
#12500=ORIENTED_EDGE('',*,*,#9297,.F.);
#12501=ORIENTED_EDGE('',*,*,#9320,.F.);
#12502=ORIENTED_EDGE('',*,*,#9298,.F.);
#12503=ORIENTED_EDGE('',*,*,#9326,.F.);
#12504=ORIENTED_EDGE('',*,*,#9263,.F.);
#12505=ORIENTED_EDGE('',*,*,#9327,.F.);
#12506=ORIENTED_EDGE('',*,*,#9251,.F.);
#12507=ORIENTED_EDGE('',*,*,#9328,.F.);
#12508=ORIENTED_EDGE('',*,*,#9329,.T.);
#12509=ORIENTED_EDGE('',*,*,#9330,.T.);
#12510=ORIENTED_EDGE('',*,*,#9295,.F.);
#12511=ORIENTED_EDGE('',*,*,#9286,.F.);
#12512=ORIENTED_EDGE('',*,*,#9290,.F.);
#12513=ORIENTED_EDGE('',*,*,#9293,.F.);
#12514=ORIENTED_EDGE('',*,*,#9283,.F.);
#12515=ORIENTED_EDGE('',*,*,#9274,.F.);
#12516=ORIENTED_EDGE('',*,*,#9278,.F.);
#12517=ORIENTED_EDGE('',*,*,#9281,.F.);
#12518=ORIENTED_EDGE('',*,*,#9299,.T.);
#12519=ORIENTED_EDGE('',*,*,#9330,.F.);
#12520=ORIENTED_EDGE('',*,*,#9331,.T.);
#12521=ORIENTED_EDGE('',*,*,#9307,.T.);
#12522=ORIENTED_EDGE('',*,*,#9253,.F.);
#12523=ORIENTED_EDGE('',*,*,#9327,.T.);
#12524=ORIENTED_EDGE('',*,*,#9271,.F.);
#12525=ORIENTED_EDGE('',*,*,#9325,.F.);
#12526=ORIENTED_EDGE('',*,*,#9260,.F.);
#12527=ORIENTED_EDGE('',*,*,#9324,.F.);
#12528=ORIENTED_EDGE('',*,*,#9332,.T.);
#12529=ORIENTED_EDGE('',*,*,#9328,.T.);
#12530=ORIENTED_EDGE('',*,*,#9246,.F.);
#12531=ORIENTED_EDGE('',*,*,#9107,.T.);
#12532=ORIENTED_EDGE('',*,*,#9312,.F.);
#12533=ORIENTED_EDGE('',*,*,#9308,.F.);
#12534=ORIENTED_EDGE('',*,*,#9331,.F.);
#12535=ORIENTED_EDGE('',*,*,#9329,.F.);
#12536=ORIENTED_EDGE('',*,*,#9332,.F.);
#12537=ORIENTED_EDGE('',*,*,#9247,.F.);
#12538=ORIENTED_EDGE('',*,*,#9322,.F.);
#12539=ORIENTED_EDGE('',*,*,#9317,.F.);
#12540=ORIENTED_EDGE('',*,*,#9313,.F.);
#12541=ORIENTED_EDGE('',*,*,#9085,.T.);
#12542=ORIENTED_EDGE('',*,*,#9202,.F.);
#12543=ORIENTED_EDGE('',*,*,#9315,.T.);
#12544=ORIENTED_EDGE('',*,*,#9209,.F.);
#12545=ORIENTED_EDGE('',*,*,#9321,.T.);
#12546=ORIENTED_EDGE('',*,*,#9319,.T.);
#12547=ORIENTED_EDGE('',*,*,#9145,.T.);
#12548=ORIENTED_EDGE('',*,*,#9316,.T.);
#12549=ORIENTED_EDGE('',*,*,#9189,.T.);
#12550=ORIENTED_EDGE('',*,*,#9238,.T.);
#12551=ORIENTED_EDGE('',*,*,#9105,.T.);
#12552=ORIENTED_EDGE('',*,*,#9100,.T.);
#12553=ORIENTED_EDGE('',*,*,#9230,.T.);
#12554=ORIENTED_EDGE('',*,*,#9240,.F.);
#12555=ORIENTED_EDGE('',*,*,#9226,.T.);
#12556=ORIENTED_EDGE('',*,*,#9323,.T.);
#12557=ORIENTED_EDGE('',*,*,#9090,.T.);
#12558=ORIENTED_EDGE('',*,*,#9097,.T.);
#12559=ORIENTED_EDGE('',*,*,#9232,.T.);
#12560=ORIENTED_EDGE('',*,*,#9242,.T.);
#12561=ORIENTED_EDGE('',*,*,#9220,.T.);
#12562=ORIENTED_EDGE('',*,*,#9333,.T.);
#12563=ORIENTED_EDGE('',*,*,#9334,.F.);
#12564=ORIENTED_EDGE('',*,*,#9335,.T.);
#12565=ORIENTED_EDGE('',*,*,#9336,.F.);
#12566=ORIENTED_EDGE('',*,*,#9337,.T.);
#12567=ORIENTED_EDGE('',*,*,#9338,.T.);
#12568=ORIENTED_EDGE('',*,*,#9339,.T.);
#12569=ORIENTED_EDGE('',*,*,#9340,.T.);
#12570=ORIENTED_EDGE('',*,*,#9341,.F.);
#12571=ORIENTED_EDGE('',*,*,#9342,.T.);
#12572=ORIENTED_EDGE('',*,*,#9343,.T.);
#12573=ORIENTED_EDGE('',*,*,#9344,.T.);
#12574=ORIENTED_EDGE('',*,*,#9345,.F.);
#12575=ORIENTED_EDGE('',*,*,#9346,.F.);
#12576=ORIENTED_EDGE('',*,*,#9347,.T.);
#12577=ORIENTED_EDGE('',*,*,#9348,.T.);
#12578=ORIENTED_EDGE('',*,*,#9349,.T.);
#12579=ORIENTED_EDGE('',*,*,#9350,.F.);
#12580=ORIENTED_EDGE('',*,*,#9351,.T.);
#12581=ORIENTED_EDGE('',*,*,#9352,.T.);
#12582=ORIENTED_EDGE('',*,*,#9353,.T.);
#12583=ORIENTED_EDGE('',*,*,#9354,.T.);
#12584=ORIENTED_EDGE('',*,*,#9355,.T.);
#12585=ORIENTED_EDGE('',*,*,#9356,.F.);
#12586=ORIENTED_EDGE('',*,*,#9357,.F.);
#12587=ORIENTED_EDGE('',*,*,#9358,.T.);
#12588=ORIENTED_EDGE('',*,*,#9359,.T.);
#12589=ORIENTED_EDGE('',*,*,#9360,.T.);
#12590=ORIENTED_EDGE('',*,*,#9361,.T.);
#12591=ORIENTED_EDGE('',*,*,#9362,.T.);
#12592=ORIENTED_EDGE('',*,*,#9363,.F.);
#12593=ORIENTED_EDGE('',*,*,#9364,.T.);
#12594=ORIENTED_EDGE('',*,*,#9365,.F.);
#12595=ORIENTED_EDGE('',*,*,#9366,.T.);
#12596=ORIENTED_EDGE('',*,*,#9367,.F.);
#12597=ORIENTED_EDGE('',*,*,#9368,.T.);
#12598=ORIENTED_EDGE('',*,*,#9369,.F.);
#12599=ORIENTED_EDGE('',*,*,#9368,.F.);
#12600=ORIENTED_EDGE('',*,*,#9370,.F.);
#12601=ORIENTED_EDGE('',*,*,#9371,.F.);
#12602=ORIENTED_EDGE('',*,*,#9372,.T.);
#12603=ORIENTED_EDGE('',*,*,#9373,.F.);
#12604=ORIENTED_EDGE('',*,*,#9372,.F.);
#12605=ORIENTED_EDGE('',*,*,#9374,.F.);
#12606=ORIENTED_EDGE('',*,*,#9375,.T.);
#12607=ORIENTED_EDGE('',*,*,#9376,.F.);
#12608=ORIENTED_EDGE('',*,*,#9377,.F.);
#12609=ORIENTED_EDGE('',*,*,#9375,.F.);
#12610=ORIENTED_EDGE('',*,*,#9378,.F.);
#12611=ORIENTED_EDGE('',*,*,#9379,.T.);
#12612=ORIENTED_EDGE('',*,*,#9380,.F.);
#12613=ORIENTED_EDGE('',*,*,#9379,.F.);
#12614=ORIENTED_EDGE('',*,*,#9381,.F.);
#12615=ORIENTED_EDGE('',*,*,#9382,.T.);
#12616=ORIENTED_EDGE('',*,*,#9383,.F.);
#12617=ORIENTED_EDGE('',*,*,#9384,.F.);
#12618=ORIENTED_EDGE('',*,*,#9382,.F.);
#12619=ORIENTED_EDGE('',*,*,#9385,.F.);
#12620=ORIENTED_EDGE('',*,*,#9386,.T.);
#12621=ORIENTED_EDGE('',*,*,#9387,.F.);
#12622=ORIENTED_EDGE('',*,*,#9386,.F.);
#12623=ORIENTED_EDGE('',*,*,#9388,.F.);
#12624=ORIENTED_EDGE('',*,*,#9389,.T.);
#12625=ORIENTED_EDGE('',*,*,#9390,.F.);
#12626=ORIENTED_EDGE('',*,*,#9389,.F.);
#12627=ORIENTED_EDGE('',*,*,#9391,.F.);
#12628=ORIENTED_EDGE('',*,*,#9392,.T.);
#12629=ORIENTED_EDGE('',*,*,#9393,.F.);
#12630=ORIENTED_EDGE('',*,*,#9392,.F.);
#12631=ORIENTED_EDGE('',*,*,#9394,.F.);
#12632=ORIENTED_EDGE('',*,*,#9395,.T.);
#12633=ORIENTED_EDGE('',*,*,#9396,.F.);
#12634=ORIENTED_EDGE('',*,*,#9395,.F.);
#12635=ORIENTED_EDGE('',*,*,#9370,.T.);
#12636=ORIENTED_EDGE('',*,*,#9371,.T.);
#12637=ORIENTED_EDGE('',*,*,#9397,.T.);
#12638=ORIENTED_EDGE('',*,*,#9385,.T.);
#12639=ORIENTED_EDGE('',*,*,#9397,.F.);
#12640=ORIENTED_EDGE('',*,*,#9390,.T.);
#12641=ORIENTED_EDGE('',*,*,#9398,.T.);
#12642=ORIENTED_EDGE('',*,*,#9399,.F.);
#12643=ORIENTED_EDGE('',*,*,#9400,.F.);
#12644=ORIENTED_EDGE('',*,*,#9401,.F.);
#12645=ORIENTED_EDGE('',*,*,#9402,.T.);
#12646=ORIENTED_EDGE('',*,*,#9403,.F.);
#12647=ORIENTED_EDGE('',*,*,#9355,.F.);
#12648=ORIENTED_EDGE('',*,*,#9404,.F.);
#12649=ORIENTED_EDGE('',*,*,#9349,.F.);
#12650=ORIENTED_EDGE('',*,*,#9405,.F.);
#12651=ORIENTED_EDGE('',*,*,#9406,.T.);
#12652=ORIENTED_EDGE('',*,*,#9407,.F.);
#12653=ORIENTED_EDGE('',*,*,#9408,.F.);
#12654=ORIENTED_EDGE('',*,*,#9409,.F.);
#12655=ORIENTED_EDGE('',*,*,#9410,.F.);
#12656=ORIENTED_EDGE('',*,*,#9411,.F.);
#12657=ORIENTED_EDGE('',*,*,#9412,.T.);
#12658=ORIENTED_EDGE('',*,*,#9413,.F.);
#12659=ORIENTED_EDGE('',*,*,#9342,.F.);
#12660=ORIENTED_EDGE('',*,*,#9414,.F.);
#12661=ORIENTED_EDGE('',*,*,#9415,.F.);
#12662=ORIENTED_EDGE('',*,*,#9416,.F.);
#12663=ORIENTED_EDGE('',*,*,#9417,.T.);
#12664=ORIENTED_EDGE('',*,*,#9418,.F.);
#12665=ORIENTED_EDGE('',*,*,#9419,.F.);
#12666=ORIENTED_EDGE('',*,*,#9420,.F.);
#12667=ORIENTED_EDGE('',*,*,#9358,.F.);
#12668=ORIENTED_EDGE('',*,*,#9421,.F.);
#12669=ORIENTED_EDGE('',*,*,#9422,.T.);
#12670=ORIENTED_EDGE('',*,*,#9423,.F.);
#12671=ORIENTED_EDGE('',*,*,#9424,.F.);
#12672=ORIENTED_EDGE('',*,*,#9425,.F.);
#12673=ORIENTED_EDGE('',*,*,#9398,.F.);
#12674=ORIENTED_EDGE('',*,*,#9426,.T.);
#12675=ORIENTED_EDGE('',*,*,#9427,.F.);
#12676=ORIENTED_EDGE('',*,*,#9406,.F.);
#12677=ORIENTED_EDGE('',*,*,#9428,.F.);
#12678=ORIENTED_EDGE('',*,*,#9429,.T.);
#12679=ORIENTED_EDGE('',*,*,#9430,.F.);
#12680=ORIENTED_EDGE('',*,*,#9402,.F.);
#12681=ORIENTED_EDGE('',*,*,#9431,.F.);
#12682=ORIENTED_EDGE('',*,*,#9432,.T.);
#12683=ORIENTED_EDGE('',*,*,#9433,.T.);
#12684=ORIENTED_EDGE('',*,*,#9434,.T.);
#12685=ORIENTED_EDGE('',*,*,#9391,.T.);
#12686=ORIENTED_EDGE('',*,*,#9434,.F.);
#12687=ORIENTED_EDGE('',*,*,#9435,.T.);
#12688=ORIENTED_EDGE('',*,*,#9436,.F.);
#12689=ORIENTED_EDGE('',*,*,#9422,.F.);
#12690=ORIENTED_EDGE('',*,*,#9437,.F.);
#12691=ORIENTED_EDGE('',*,*,#9438,.T.);
#12692=ORIENTED_EDGE('',*,*,#9439,.F.);
#12693=ORIENTED_EDGE('',*,*,#9417,.F.);
#12694=ORIENTED_EDGE('',*,*,#9440,.F.);
#12695=ORIENTED_EDGE('',*,*,#9441,.T.);
#12696=ORIENTED_EDGE('',*,*,#9442,.F.);
#12697=ORIENTED_EDGE('',*,*,#9412,.F.);
#12698=ORIENTED_EDGE('',*,*,#9443,.F.);
#12699=ORIENTED_EDGE('',*,*,#9393,.T.);
#12700=ORIENTED_EDGE('',*,*,#9394,.T.);
#12701=ORIENTED_EDGE('',*,*,#9396,.T.);
#12702=ORIENTED_EDGE('',*,*,#9444,.T.);
#12703=ORIENTED_EDGE('',*,*,#9367,.T.);
#12704=ORIENTED_EDGE('',*,*,#9444,.F.);
#12705=ORIENTED_EDGE('',*,*,#9369,.T.);
#12706=ORIENTED_EDGE('',*,*,#9378,.T.);
#12707=ORIENTED_EDGE('',*,*,#9380,.T.);
#12708=ORIENTED_EDGE('',*,*,#9445,.T.);
#12709=ORIENTED_EDGE('',*,*,#9383,.T.);
#12710=ORIENTED_EDGE('',*,*,#9384,.T.);
#12711=ORIENTED_EDGE('',*,*,#9445,.F.);
#12712=ORIENTED_EDGE('',*,*,#9446,.T.);
#12713=ORIENTED_EDGE('',*,*,#9381,.T.);
#12714=ORIENTED_EDGE('',*,*,#9446,.F.);
#12715=ORIENTED_EDGE('',*,*,#9447,.T.);
#12716=ORIENTED_EDGE('',*,*,#9374,.T.);
#12717=ORIENTED_EDGE('',*,*,#9447,.F.);
#12718=ORIENTED_EDGE('',*,*,#9373,.T.);
#12719=ORIENTED_EDGE('',*,*,#9448,.T.);
#12720=ORIENTED_EDGE('',*,*,#9376,.T.);
#12721=ORIENTED_EDGE('',*,*,#9377,.T.);
#12722=ORIENTED_EDGE('',*,*,#9448,.F.);
#12723=ORIENTED_EDGE('',*,*,#9387,.T.);
#12724=ORIENTED_EDGE('',*,*,#9388,.T.);
#12725=ORIENTED_EDGE('',*,*,#9449,.F.);
#12726=ORIENTED_EDGE('',*,*,#9450,.F.);
#12727=ORIENTED_EDGE('',*,*,#9451,.T.);
#12728=ORIENTED_EDGE('',*,*,#9452,.F.);
#12729=ORIENTED_EDGE('',*,*,#9451,.F.);
#12730=ORIENTED_EDGE('',*,*,#9453,.F.);
#12731=ORIENTED_EDGE('',*,*,#9454,.T.);
#12732=ORIENTED_EDGE('',*,*,#9455,.F.);
#12733=ORIENTED_EDGE('',*,*,#9454,.F.);
#12734=ORIENTED_EDGE('',*,*,#9456,.F.);
#12735=ORIENTED_EDGE('',*,*,#9457,.F.);
#12736=ORIENTED_EDGE('',*,*,#9458,.T.);
#12737=ORIENTED_EDGE('',*,*,#9459,.F.);
#12738=ORIENTED_EDGE('',*,*,#9458,.F.);
#12739=ORIENTED_EDGE('',*,*,#9365,.T.);
#12740=ORIENTED_EDGE('',*,*,#9460,.F.);
#12741=ORIENTED_EDGE('',*,*,#9461,.T.);
#12742=ORIENTED_EDGE('',*,*,#9462,.F.);
#12743=ORIENTED_EDGE('',*,*,#9463,.T.);
#12744=ORIENTED_EDGE('',*,*,#9461,.F.);
#12745=ORIENTED_EDGE('',*,*,#9464,.T.);
#12746=ORIENTED_EDGE('',*,*,#9424,.T.);
#12747=ORIENTED_EDGE('',*,*,#9399,.T.);
#12748=ORIENTED_EDGE('',*,*,#9425,.T.);
#12749=ORIENTED_EDGE('',*,*,#9464,.F.);
#12750=ORIENTED_EDGE('',*,*,#9465,.F.);
#12751=ORIENTED_EDGE('',*,*,#9466,.T.);
#12752=ORIENTED_EDGE('',*,*,#9423,.T.);
#12753=ORIENTED_EDGE('',*,*,#9436,.T.);
#12754=ORIENTED_EDGE('',*,*,#9467,.F.);
#12755=ORIENTED_EDGE('',*,*,#9468,.T.);
#12756=ORIENTED_EDGE('',*,*,#9469,.F.);
#12757=ORIENTED_EDGE('',*,*,#9470,.F.);
#12758=ORIENTED_EDGE('',*,*,#9463,.F.);
#12759=ORIENTED_EDGE('',*,*,#9471,.T.);
#12760=ORIENTED_EDGE('',*,*,#9472,.F.);
#12761=ORIENTED_EDGE('',*,*,#9366,.F.);
#12762=ORIENTED_EDGE('',*,*,#9473,.F.);
#12763=ORIENTED_EDGE('',*,*,#9474,.F.);
#12764=ORIENTED_EDGE('',*,*,#9475,.F.);
#12765=ORIENTED_EDGE('',*,*,#9364,.F.);
#12766=ORIENTED_EDGE('',*,*,#9476,.F.);
#12767=ORIENTED_EDGE('',*,*,#9363,.T.);
#12768=ORIENTED_EDGE('',*,*,#9477,.T.);
#12769=ORIENTED_EDGE('',*,*,#9400,.T.);
#12770=ORIENTED_EDGE('',*,*,#9466,.F.);
#12771=ORIENTED_EDGE('',*,*,#9478,.T.);
#12772=ORIENTED_EDGE('',*,*,#9479,.T.);
#12773=ORIENTED_EDGE('',*,*,#9480,.F.);
#12774=ORIENTED_EDGE('',*,*,#9468,.F.);
#12775=ORIENTED_EDGE('',*,*,#9481,.F.);
#12776=ORIENTED_EDGE('',*,*,#9482,.T.);
#12777=ORIENTED_EDGE('',*,*,#9483,.F.);
#12778=ORIENTED_EDGE('',*,*,#9471,.F.);
#12779=ORIENTED_EDGE('',*,*,#9484,.F.);
#12780=ORIENTED_EDGE('',*,*,#9362,.F.);
#12781=ORIENTED_EDGE('',*,*,#9485,.F.);
#12782=ORIENTED_EDGE('',*,*,#9478,.F.);
#12783=ORIENTED_EDGE('',*,*,#9486,.F.);
#12784=ORIENTED_EDGE('',*,*,#9431,.T.);
#12785=ORIENTED_EDGE('',*,*,#9401,.T.);
#12786=ORIENTED_EDGE('',*,*,#9477,.F.);
#12787=ORIENTED_EDGE('',*,*,#9487,.F.);
#12788=ORIENTED_EDGE('',*,*,#9488,.F.);
#12789=ORIENTED_EDGE('',*,*,#9489,.T.);
#12790=ORIENTED_EDGE('',*,*,#9490,.F.);
#12791=ORIENTED_EDGE('',*,*,#9491,.F.);
#12792=ORIENTED_EDGE('',*,*,#9437,.T.);
#12793=ORIENTED_EDGE('',*,*,#9421,.T.);
#12794=ORIENTED_EDGE('',*,*,#9357,.T.);
#12795=ORIENTED_EDGE('',*,*,#9492,.F.);
#12796=ORIENTED_EDGE('',*,*,#9493,.F.);
#12797=ORIENTED_EDGE('',*,*,#9479,.F.);
#12798=ORIENTED_EDGE('',*,*,#9494,.T.);
#12799=ORIENTED_EDGE('',*,*,#9495,.F.);
#12800=ORIENTED_EDGE('',*,*,#9482,.F.);
#12801=ORIENTED_EDGE('',*,*,#9496,.F.);
#12802=ORIENTED_EDGE('',*,*,#9497,.F.);
#12803=ORIENTED_EDGE('',*,*,#9498,.F.);
#12804=ORIENTED_EDGE('',*,*,#9499,.F.);
#12805=ORIENTED_EDGE('',*,*,#9361,.F.);
#12806=ORIENTED_EDGE('',*,*,#9500,.F.);
#12807=ORIENTED_EDGE('',*,*,#9501,.T.);
#12808=ORIENTED_EDGE('',*,*,#9502,.T.);
#12809=ORIENTED_EDGE('',*,*,#9503,.F.);
#12810=ORIENTED_EDGE('',*,*,#9489,.F.);
#12811=ORIENTED_EDGE('',*,*,#9504,.F.);
#12812=ORIENTED_EDGE('',*,*,#9505,.T.);
#12813=ORIENTED_EDGE('',*,*,#9494,.F.);
#12814=ORIENTED_EDGE('',*,*,#9506,.T.);
#12815=ORIENTED_EDGE('',*,*,#9507,.F.);
#12816=ORIENTED_EDGE('',*,*,#9501,.F.);
#12817=ORIENTED_EDGE('',*,*,#9508,.F.);
#12818=ORIENTED_EDGE('',*,*,#9509,.T.);
#12819=ORIENTED_EDGE('',*,*,#9356,.T.);
#12820=ORIENTED_EDGE('',*,*,#9403,.T.);
#12821=ORIENTED_EDGE('',*,*,#9430,.T.);
#12822=ORIENTED_EDGE('',*,*,#9510,.F.);
#12823=ORIENTED_EDGE('',*,*,#9502,.F.);
#12824=ORIENTED_EDGE('',*,*,#9511,.F.);
#12825=ORIENTED_EDGE('',*,*,#9512,.F.);
#12826=ORIENTED_EDGE('',*,*,#9359,.F.);
#12827=ORIENTED_EDGE('',*,*,#9420,.T.);
#12828=ORIENTED_EDGE('',*,*,#9513,.T.);
#12829=ORIENTED_EDGE('',*,*,#9514,.F.);
#12830=ORIENTED_EDGE('',*,*,#9360,.F.);
#12831=ORIENTED_EDGE('',*,*,#9515,.F.);
#12832=ORIENTED_EDGE('',*,*,#9506,.F.);
#12833=ORIENTED_EDGE('',*,*,#9516,.F.);
#12834=ORIENTED_EDGE('',*,*,#9350,.T.);
#12835=ORIENTED_EDGE('',*,*,#9517,.F.);
#12836=ORIENTED_EDGE('',*,*,#9505,.F.);
#12837=ORIENTED_EDGE('',*,*,#9518,.F.);
#12838=ORIENTED_EDGE('',*,*,#9519,.T.);
#12839=ORIENTED_EDGE('',*,*,#9520,.F.);
#12840=ORIENTED_EDGE('',*,*,#9521,.F.);
#12841=ORIENTED_EDGE('',*,*,#9509,.F.);
#12842=ORIENTED_EDGE('',*,*,#9522,.F.);
#12843=ORIENTED_EDGE('',*,*,#9513,.F.);
#12844=ORIENTED_EDGE('',*,*,#9419,.T.);
#12845=ORIENTED_EDGE('',*,*,#9523,.T.);
#12846=ORIENTED_EDGE('',*,*,#9524,.T.);
#12847=ORIENTED_EDGE('',*,*,#9525,.T.);
#12848=ORIENTED_EDGE('',*,*,#9519,.F.);
#12849=ORIENTED_EDGE('',*,*,#9526,.T.);
#12850=ORIENTED_EDGE('',*,*,#9525,.F.);
#12851=ORIENTED_EDGE('',*,*,#9527,.F.);
#12852=ORIENTED_EDGE('',*,*,#9353,.F.);
#12853=ORIENTED_EDGE('',*,*,#9528,.F.);
#12854=ORIENTED_EDGE('',*,*,#9346,.T.);
#12855=ORIENTED_EDGE('',*,*,#9404,.T.);
#12856=ORIENTED_EDGE('',*,*,#9354,.F.);
#12857=ORIENTED_EDGE('',*,*,#9529,.F.);
#12858=ORIENTED_EDGE('',*,*,#9418,.T.);
#12859=ORIENTED_EDGE('',*,*,#9439,.T.);
#12860=ORIENTED_EDGE('',*,*,#9530,.F.);
#12861=ORIENTED_EDGE('',*,*,#9531,.T.);
#12862=ORIENTED_EDGE('',*,*,#9532,.F.);
#12863=ORIENTED_EDGE('',*,*,#9533,.F.);
#12864=ORIENTED_EDGE('',*,*,#9523,.F.);
#12865=ORIENTED_EDGE('',*,*,#9524,.F.);
#12866=ORIENTED_EDGE('',*,*,#9534,.F.);
#12867=ORIENTED_EDGE('',*,*,#9351,.F.);
#12868=ORIENTED_EDGE('',*,*,#9535,.F.);
#12869=ORIENTED_EDGE('',*,*,#9536,.T.);
#12870=ORIENTED_EDGE('',*,*,#9537,.F.);
#12871=ORIENTED_EDGE('',*,*,#9352,.F.);
#12872=ORIENTED_EDGE('',*,*,#9538,.F.);
#12873=ORIENTED_EDGE('',*,*,#9539,.F.);
#12874=ORIENTED_EDGE('',*,*,#9540,.T.);
#12875=ORIENTED_EDGE('',*,*,#9541,.F.);
#12876=ORIENTED_EDGE('',*,*,#9526,.F.);
#12877=ORIENTED_EDGE('',*,*,#9542,.F.);
#12878=ORIENTED_EDGE('',*,*,#9543,.T.);
#12879=ORIENTED_EDGE('',*,*,#9544,.F.);
#12880=ORIENTED_EDGE('',*,*,#9531,.F.);
#12881=ORIENTED_EDGE('',*,*,#9545,.F.);
#12882=ORIENTED_EDGE('',*,*,#9546,.T.);
#12883=ORIENTED_EDGE('',*,*,#9547,.F.);
#12884=ORIENTED_EDGE('',*,*,#9536,.F.);
#12885=ORIENTED_EDGE('',*,*,#9548,.F.);
#12886=ORIENTED_EDGE('',*,*,#9549,.T.);
#12887=ORIENTED_EDGE('',*,*,#9550,.T.);
#12888=ORIENTED_EDGE('',*,*,#9540,.F.);
#12889=ORIENTED_EDGE('',*,*,#9550,.F.);
#12890=ORIENTED_EDGE('',*,*,#9551,.F.);
#12891=ORIENTED_EDGE('',*,*,#9347,.F.);
#12892=ORIENTED_EDGE('',*,*,#9552,.F.);
#12893=ORIENTED_EDGE('',*,*,#9428,.T.);
#12894=ORIENTED_EDGE('',*,*,#9405,.T.);
#12895=ORIENTED_EDGE('',*,*,#9348,.F.);
#12896=ORIENTED_EDGE('',*,*,#9553,.F.);
#12897=ORIENTED_EDGE('',*,*,#9554,.F.);
#12898=ORIENTED_EDGE('',*,*,#9555,.T.);
#12899=ORIENTED_EDGE('',*,*,#9556,.F.);
#12900=ORIENTED_EDGE('',*,*,#9557,.F.);
#12901=ORIENTED_EDGE('',*,*,#9440,.T.);
#12902=ORIENTED_EDGE('',*,*,#9416,.T.);
#12903=ORIENTED_EDGE('',*,*,#9558,.T.);
#12904=ORIENTED_EDGE('',*,*,#9559,.F.);
#12905=ORIENTED_EDGE('',*,*,#9560,.F.);
#12906=ORIENTED_EDGE('',*,*,#9543,.F.);
#12907=ORIENTED_EDGE('',*,*,#9345,.T.);
#12908=ORIENTED_EDGE('',*,*,#9561,.F.);
#12909=ORIENTED_EDGE('',*,*,#9546,.F.);
#12910=ORIENTED_EDGE('',*,*,#9562,.F.);
#12911=ORIENTED_EDGE('',*,*,#9563,.F.);
#12912=ORIENTED_EDGE('',*,*,#9564,.F.);
#12913=ORIENTED_EDGE('',*,*,#9565,.F.);
#12914=ORIENTED_EDGE('',*,*,#9549,.F.);
#12915=ORIENTED_EDGE('',*,*,#9566,.F.);
#12916=ORIENTED_EDGE('',*,*,#9567,.T.);
#12917=ORIENTED_EDGE('',*,*,#9568,.T.);
#12918=ORIENTED_EDGE('',*,*,#9569,.F.);
#12919=ORIENTED_EDGE('',*,*,#9555,.F.);
#12920=ORIENTED_EDGE('',*,*,#9570,.F.);
#12921=ORIENTED_EDGE('',*,*,#9558,.F.);
#12922=ORIENTED_EDGE('',*,*,#9415,.T.);
#12923=ORIENTED_EDGE('',*,*,#9571,.T.);
#12924=ORIENTED_EDGE('',*,*,#9572,.T.);
#12925=ORIENTED_EDGE('',*,*,#9573,.F.);
#12926=ORIENTED_EDGE('',*,*,#9567,.F.);
#12927=ORIENTED_EDGE('',*,*,#9574,.F.);
#12928=ORIENTED_EDGE('',*,*,#9575,.T.);
#12929=ORIENTED_EDGE('',*,*,#9576,.T.);
#12930=ORIENTED_EDGE('',*,*,#9407,.T.);
#12931=ORIENTED_EDGE('',*,*,#9427,.T.);
#12932=ORIENTED_EDGE('',*,*,#9577,.F.);
#12933=ORIENTED_EDGE('',*,*,#9568,.F.);
#12934=ORIENTED_EDGE('',*,*,#9578,.F.);
#12935=ORIENTED_EDGE('',*,*,#9579,.F.);
#12936=ORIENTED_EDGE('',*,*,#9571,.F.);
#12937=ORIENTED_EDGE('',*,*,#9414,.T.);
#12938=ORIENTED_EDGE('',*,*,#9341,.T.);
#12939=ORIENTED_EDGE('',*,*,#9580,.F.);
#12940=ORIENTED_EDGE('',*,*,#9572,.F.);
#12941=ORIENTED_EDGE('',*,*,#9581,.F.);
#12942=ORIENTED_EDGE('',*,*,#9343,.F.);
#12943=ORIENTED_EDGE('',*,*,#9582,.F.);
#12944=ORIENTED_EDGE('',*,*,#9583,.T.);
#12945=ORIENTED_EDGE('',*,*,#9584,.F.);
#12946=ORIENTED_EDGE('',*,*,#9344,.F.);
#12947=ORIENTED_EDGE('',*,*,#9585,.F.);
#12948=ORIENTED_EDGE('',*,*,#9586,.F.);
#12949=ORIENTED_EDGE('',*,*,#9587,.F.);
#12950=ORIENTED_EDGE('',*,*,#9575,.F.);
#12951=ORIENTED_EDGE('',*,*,#9588,.F.);
#12952=ORIENTED_EDGE('',*,*,#9336,.T.);
#12953=ORIENTED_EDGE('',*,*,#9589,.T.);
#12954=ORIENTED_EDGE('',*,*,#9408,.T.);
#12955=ORIENTED_EDGE('',*,*,#9576,.F.);
#12956=ORIENTED_EDGE('',*,*,#9590,.T.);
#12957=ORIENTED_EDGE('',*,*,#9591,.T.);
#12958=ORIENTED_EDGE('',*,*,#9583,.F.);
#12959=ORIENTED_EDGE('',*,*,#9592,.T.);
#12960=ORIENTED_EDGE('',*,*,#9338,.F.);
#12961=ORIENTED_EDGE('',*,*,#9593,.F.);
#12962=ORIENTED_EDGE('',*,*,#9590,.F.);
#12963=ORIENTED_EDGE('',*,*,#9594,.F.);
#12964=ORIENTED_EDGE('',*,*,#9409,.T.);
#12965=ORIENTED_EDGE('',*,*,#9589,.F.);
#12966=ORIENTED_EDGE('',*,*,#9595,.F.);
#12967=ORIENTED_EDGE('',*,*,#9596,.T.);
#12968=ORIENTED_EDGE('',*,*,#9413,.T.);
#12969=ORIENTED_EDGE('',*,*,#9442,.T.);
#12970=ORIENTED_EDGE('',*,*,#9597,.F.);
#12971=ORIENTED_EDGE('',*,*,#9598,.T.);
#12972=ORIENTED_EDGE('',*,*,#9599,.F.);
#12973=ORIENTED_EDGE('',*,*,#9600,.F.);
#12974=ORIENTED_EDGE('',*,*,#9339,.F.);
#12975=ORIENTED_EDGE('',*,*,#9340,.F.);
#12976=ORIENTED_EDGE('',*,*,#9601,.F.);
#12977=ORIENTED_EDGE('',*,*,#9592,.F.);
#12978=ORIENTED_EDGE('',*,*,#9602,.F.);
#12979=ORIENTED_EDGE('',*,*,#9603,.T.);
#12980=ORIENTED_EDGE('',*,*,#9604,.F.);
#12981=ORIENTED_EDGE('',*,*,#9591,.F.);
#12982=ORIENTED_EDGE('',*,*,#9605,.F.);
#12983=ORIENTED_EDGE('',*,*,#9606,.F.);
#12984=ORIENTED_EDGE('',*,*,#9334,.T.);
#12985=ORIENTED_EDGE('',*,*,#9607,.F.);
#12986=ORIENTED_EDGE('',*,*,#9337,.F.);
#12987=ORIENTED_EDGE('',*,*,#9608,.F.);
#12988=ORIENTED_EDGE('',*,*,#9609,.F.);
#12989=ORIENTED_EDGE('',*,*,#9610,.T.);
#12990=ORIENTED_EDGE('',*,*,#9611,.T.);
#12991=ORIENTED_EDGE('',*,*,#9410,.T.);
#12992=ORIENTED_EDGE('',*,*,#9596,.F.);
#12993=ORIENTED_EDGE('',*,*,#9612,.T.);
#12994=ORIENTED_EDGE('',*,*,#9613,.F.);
#12995=ORIENTED_EDGE('',*,*,#9598,.F.);
#12996=ORIENTED_EDGE('',*,*,#9614,.F.);
#12997=ORIENTED_EDGE('',*,*,#9615,.T.);
#12998=ORIENTED_EDGE('',*,*,#9616,.F.);
#12999=ORIENTED_EDGE('',*,*,#9603,.F.);
#13000=ORIENTED_EDGE('',*,*,#9617,.F.);
#13001=ORIENTED_EDGE('',*,*,#9333,.F.);
#13002=ORIENTED_EDGE('',*,*,#9618,.F.);
#13003=ORIENTED_EDGE('',*,*,#9610,.F.);
#13004=ORIENTED_EDGE('',*,*,#9619,.F.);
#13005=ORIENTED_EDGE('',*,*,#9620,.F.);
#13006=ORIENTED_EDGE('',*,*,#9443,.T.);
#13007=ORIENTED_EDGE('',*,*,#9411,.T.);
#13008=ORIENTED_EDGE('',*,*,#9611,.F.);
#13009=ORIENTED_EDGE('',*,*,#9621,.F.);
#13010=ORIENTED_EDGE('',*,*,#9622,.F.);
#13011=ORIENTED_EDGE('',*,*,#9612,.F.);
#13012=ORIENTED_EDGE('',*,*,#9623,.F.);
#13013=ORIENTED_EDGE('',*,*,#9624,.F.);
#13014=ORIENTED_EDGE('',*,*,#9335,.F.);
#13015=ORIENTED_EDGE('',*,*,#9625,.F.);
#13016=ORIENTED_EDGE('',*,*,#9615,.F.);
#13017=ORIENTED_EDGE('',*,*,#9626,.F.);
#13018=ORIENTED_EDGE('',*,*,#9627,.T.);
#13019=ORIENTED_EDGE('',*,*,#9628,.F.);
#13020=ORIENTED_EDGE('',*,*,#9627,.F.);
#13021=ORIENTED_EDGE('',*,*,#9629,.T.);
#13022=ORIENTED_EDGE('',*,*,#9532,.T.);
#13023=ORIENTED_EDGE('',*,*,#9544,.T.);
#13024=ORIENTED_EDGE('',*,*,#9560,.T.);
#13025=ORIENTED_EDGE('',*,*,#9630,.T.);
#13026=ORIENTED_EDGE('',*,*,#9562,.T.);
#13027=ORIENTED_EDGE('',*,*,#9548,.T.);
#13028=ORIENTED_EDGE('',*,*,#9539,.T.);
#13029=ORIENTED_EDGE('',*,*,#9630,.F.);
#13030=ORIENTED_EDGE('',*,*,#9559,.T.);
#13031=ORIENTED_EDGE('',*,*,#9582,.T.);
#13032=ORIENTED_EDGE('',*,*,#9563,.T.);
#13033=ORIENTED_EDGE('',*,*,#9534,.T.);
#13034=ORIENTED_EDGE('',*,*,#9533,.T.);
#13035=ORIENTED_EDGE('',*,*,#9629,.F.);
#13036=ORIENTED_EDGE('',*,*,#9538,.T.);
#13037=ORIENTED_EDGE('',*,*,#9631,.T.);
#13038=ORIENTED_EDGE('',*,*,#9599,.T.);
#13039=ORIENTED_EDGE('',*,*,#9613,.T.);
#13040=ORIENTED_EDGE('',*,*,#9622,.T.);
#13041=ORIENTED_EDGE('',*,*,#9632,.T.);
#13042=ORIENTED_EDGE('',*,*,#9623,.T.);
#13043=ORIENTED_EDGE('',*,*,#9617,.T.);
#13044=ORIENTED_EDGE('',*,*,#9606,.T.);
#13045=ORIENTED_EDGE('',*,*,#9601,.T.);
#13046=ORIENTED_EDGE('',*,*,#9600,.T.);
#13047=ORIENTED_EDGE('',*,*,#9631,.F.);
#13048=ORIENTED_EDGE('',*,*,#9605,.T.);
#13049=ORIENTED_EDGE('',*,*,#9632,.F.);
#13050=ORIENTED_EDGE('',*,*,#9621,.T.);
#13051=ORIENTED_EDGE('',*,*,#9618,.T.);
#13052=ORIENTED_EDGE('',*,*,#9624,.T.);
#13053=ORIENTED_EDGE('',*,*,#9633,.T.);
#13054=ORIENTED_EDGE('',*,*,#9578,.T.);
#13055=ORIENTED_EDGE('',*,*,#9570,.T.);
#13056=ORIENTED_EDGE('',*,*,#9554,.T.);
#13057=ORIENTED_EDGE('',*,*,#9634,.T.);
#13058=ORIENTED_EDGE('',*,*,#9564,.T.);
#13059=ORIENTED_EDGE('',*,*,#9573,.T.);
#13060=ORIENTED_EDGE('',*,*,#9587,.T.);
#13061=ORIENTED_EDGE('',*,*,#9594,.T.);
#13062=ORIENTED_EDGE('',*,*,#9579,.T.);
#13063=ORIENTED_EDGE('',*,*,#9633,.F.);
#13064=ORIENTED_EDGE('',*,*,#9586,.T.);
#13065=ORIENTED_EDGE('',*,*,#9634,.F.);
#13066=ORIENTED_EDGE('',*,*,#9553,.T.);
#13067=ORIENTED_EDGE('',*,*,#9551,.T.);
#13068=ORIENTED_EDGE('',*,*,#9565,.T.);
#13069=ORIENTED_EDGE('',*,*,#9635,.T.);
#13070=ORIENTED_EDGE('',*,*,#9511,.T.);
#13071=ORIENTED_EDGE('',*,*,#9504,.T.);
#13072=ORIENTED_EDGE('',*,*,#9488,.T.);
#13073=ORIENTED_EDGE('',*,*,#9636,.T.);
#13074=ORIENTED_EDGE('',*,*,#9498,.T.);
#13075=ORIENTED_EDGE('',*,*,#9507,.T.);
#13076=ORIENTED_EDGE('',*,*,#9521,.T.);
#13077=ORIENTED_EDGE('',*,*,#9528,.T.);
#13078=ORIENTED_EDGE('',*,*,#9512,.T.);
#13079=ORIENTED_EDGE('',*,*,#9635,.F.);
#13080=ORIENTED_EDGE('',*,*,#9520,.T.);
#13081=ORIENTED_EDGE('',*,*,#9636,.F.);
#13082=ORIENTED_EDGE('',*,*,#9487,.T.);
#13083=ORIENTED_EDGE('',*,*,#9485,.T.);
#13084=ORIENTED_EDGE('',*,*,#9499,.T.);
#13085=ORIENTED_EDGE('',*,*,#9637,.T.);
#13086=ORIENTED_EDGE('',*,*,#9469,.T.);
#13087=ORIENTED_EDGE('',*,*,#9480,.T.);
#13088=ORIENTED_EDGE('',*,*,#9493,.T.);
#13089=ORIENTED_EDGE('',*,*,#9638,.T.);
#13090=ORIENTED_EDGE('',*,*,#9496,.T.);
#13091=ORIENTED_EDGE('',*,*,#9484,.T.);
#13092=ORIENTED_EDGE('',*,*,#9474,.T.);
#13093=ORIENTED_EDGE('',*,*,#9462,.T.);
#13094=ORIENTED_EDGE('',*,*,#9470,.T.);
#13095=ORIENTED_EDGE('',*,*,#9637,.F.);
#13096=ORIENTED_EDGE('',*,*,#9473,.T.);
#13097=ORIENTED_EDGE('',*,*,#9638,.F.);
#13098=ORIENTED_EDGE('',*,*,#9492,.T.);
#13099=ORIENTED_EDGE('',*,*,#9516,.T.);
#13100=ORIENTED_EDGE('',*,*,#9497,.T.);
#13101=ORIENTED_EDGE('',*,*,#9452,.T.);
#13102=ORIENTED_EDGE('',*,*,#9639,.F.);
#13103=ORIENTED_EDGE('',*,*,#9640,.F.);
#13104=ORIENTED_EDGE('',*,*,#9641,.T.);
#13105=ORIENTED_EDGE('',*,*,#9639,.T.);
#13106=ORIENTED_EDGE('',*,*,#9641,.F.);
#13107=ORIENTED_EDGE('',*,*,#9456,.T.);
#13108=ORIENTED_EDGE('',*,*,#9457,.T.);
#13109=ORIENTED_EDGE('',*,*,#9642,.T.);
#13110=ORIENTED_EDGE('',*,*,#9640,.T.);
#13111=ORIENTED_EDGE('',*,*,#9642,.F.);
#13112=ORIENTED_EDGE('',*,*,#9459,.T.);
#13113=ORIENTED_EDGE('',*,*,#9643,.T.);
#13114=ORIENTED_EDGE('',*,*,#9432,.F.);
#13115=ORIENTED_EDGE('',*,*,#9490,.T.);
#13116=ORIENTED_EDGE('',*,*,#9503,.T.);
#13117=ORIENTED_EDGE('',*,*,#9510,.T.);
#13118=ORIENTED_EDGE('',*,*,#9429,.F.);
#13119=ORIENTED_EDGE('',*,*,#9556,.T.);
#13120=ORIENTED_EDGE('',*,*,#9569,.T.);
#13121=ORIENTED_EDGE('',*,*,#9577,.T.);
#13122=ORIENTED_EDGE('',*,*,#9426,.F.);
#13123=ORIENTED_EDGE('',*,*,#9620,.T.);
#13124=ORIENTED_EDGE('',*,*,#9614,.T.);
#13125=ORIENTED_EDGE('',*,*,#9597,.T.);
#13126=ORIENTED_EDGE('',*,*,#9441,.F.);
#13127=ORIENTED_EDGE('',*,*,#9557,.T.);
#13128=ORIENTED_EDGE('',*,*,#9545,.T.);
#13129=ORIENTED_EDGE('',*,*,#9530,.T.);
#13130=ORIENTED_EDGE('',*,*,#9438,.F.);
#13131=ORIENTED_EDGE('',*,*,#9491,.T.);
#13132=ORIENTED_EDGE('',*,*,#9481,.T.);
#13133=ORIENTED_EDGE('',*,*,#9467,.T.);
#13134=ORIENTED_EDGE('',*,*,#9435,.F.);
#13135=ORIENTED_EDGE('',*,*,#9433,.F.);
#13136=ORIENTED_EDGE('',*,*,#9643,.F.);
#13137=ORIENTED_EDGE('',*,*,#9581,.T.);
#13138=ORIENTED_EDGE('',*,*,#9580,.T.);
#13139=ORIENTED_EDGE('',*,*,#9602,.T.);
#13140=ORIENTED_EDGE('',*,*,#9585,.T.);
#13141=ORIENTED_EDGE('',*,*,#9455,.T.);
#13142=ORIENTED_EDGE('',*,*,#9644,.T.);
#13143=ORIENTED_EDGE('',*,*,#9608,.T.);
#13144=ORIENTED_EDGE('',*,*,#9588,.T.);
#13145=ORIENTED_EDGE('',*,*,#9574,.T.);
#13146=ORIENTED_EDGE('',*,*,#9566,.T.);
#13147=ORIENTED_EDGE('',*,*,#9542,.T.);
#13148=ORIENTED_EDGE('',*,*,#9522,.T.);
#13149=ORIENTED_EDGE('',*,*,#9508,.T.);
#13150=ORIENTED_EDGE('',*,*,#9500,.T.);
#13151=ORIENTED_EDGE('',*,*,#9476,.T.);
#13152=ORIENTED_EDGE('',*,*,#9472,.T.);
#13153=ORIENTED_EDGE('',*,*,#9483,.T.);
#13154=ORIENTED_EDGE('',*,*,#9495,.T.);
#13155=ORIENTED_EDGE('',*,*,#9517,.T.);
#13156=ORIENTED_EDGE('',*,*,#9537,.T.);
#13157=ORIENTED_EDGE('',*,*,#9547,.T.);
#13158=ORIENTED_EDGE('',*,*,#9561,.T.);
#13159=ORIENTED_EDGE('',*,*,#9584,.T.);
#13160=ORIENTED_EDGE('',*,*,#9604,.T.);
#13161=ORIENTED_EDGE('',*,*,#9616,.T.);
#13162=ORIENTED_EDGE('',*,*,#9625,.T.);
#13163=ORIENTED_EDGE('',*,*,#9609,.T.);
#13164=ORIENTED_EDGE('',*,*,#9644,.F.);
#13165=ORIENTED_EDGE('',*,*,#9628,.T.);
#13166=ORIENTED_EDGE('',*,*,#9453,.T.);
#13167=ORIENTED_EDGE('',*,*,#9449,.T.);
#13168=ORIENTED_EDGE('',*,*,#9450,.T.);
#13169=ORIENTED_EDGE('',*,*,#9645,.T.);
#13170=ORIENTED_EDGE('',*,*,#9626,.T.);
#13171=ORIENTED_EDGE('',*,*,#9645,.F.);
#13172=ORIENTED_EDGE('',*,*,#9486,.T.);
#13173=ORIENTED_EDGE('',*,*,#9465,.T.);
#13174=ORIENTED_EDGE('',*,*,#9460,.T.);
#13175=ORIENTED_EDGE('',*,*,#9475,.T.);
#13176=ORIENTED_EDGE('',*,*,#9552,.T.);
#13177=ORIENTED_EDGE('',*,*,#9529,.T.);
#13178=ORIENTED_EDGE('',*,*,#9527,.T.);
#13179=ORIENTED_EDGE('',*,*,#9541,.T.);
#13180=ORIENTED_EDGE('',*,*,#9619,.T.);
#13181=ORIENTED_EDGE('',*,*,#9595,.T.);
#13182=ORIENTED_EDGE('',*,*,#9593,.T.);
#13183=ORIENTED_EDGE('',*,*,#9607,.T.);
#13184=ORIENTED_EDGE('',*,*,#9515,.T.);
#13185=ORIENTED_EDGE('',*,*,#9514,.T.);
#13186=ORIENTED_EDGE('',*,*,#9535,.T.);
#13187=ORIENTED_EDGE('',*,*,#9518,.T.);
#13188=ORIENTED_EDGE('',*,*,#9646,.F.);
#13189=ORIENTED_EDGE('',*,*,#9647,.F.);
#13190=ORIENTED_EDGE('',*,*,#9648,.F.);
#13191=ORIENTED_EDGE('',*,*,#9649,.F.);
#13192=ORIENTED_EDGE('',*,*,#9650,.F.);
#13193=ORIENTED_EDGE('',*,*,#9651,.F.);
#13194=ORIENTED_EDGE('',*,*,#9652,.F.);
#13195=ORIENTED_EDGE('',*,*,#9653,.F.);
#13196=ORIENTED_EDGE('',*,*,#9654,.F.);
#13197=ORIENTED_EDGE('',*,*,#9655,.F.);
#13198=ORIENTED_EDGE('',*,*,#9656,.F.);
#13199=ORIENTED_EDGE('',*,*,#9657,.F.);
#13200=ORIENTED_EDGE('',*,*,#9658,.F.);
#13201=ORIENTED_EDGE('',*,*,#9659,.F.);
#13202=ORIENTED_EDGE('',*,*,#9660,.F.);
#13203=ORIENTED_EDGE('',*,*,#9661,.F.);
#13204=ORIENTED_EDGE('',*,*,#9662,.F.);
#13205=ORIENTED_EDGE('',*,*,#9663,.F.);
#13206=ORIENTED_EDGE('',*,*,#9664,.F.);
#13207=ORIENTED_EDGE('',*,*,#9665,.F.);
#13208=ORIENTED_EDGE('',*,*,#9666,.F.);
#13209=ORIENTED_EDGE('',*,*,#9667,.F.);
#13210=ORIENTED_EDGE('',*,*,#9668,.F.);
#13211=ORIENTED_EDGE('',*,*,#9669,.F.);
#13212=ORIENTED_EDGE('',*,*,#9670,.F.);
#13213=ORIENTED_EDGE('',*,*,#9671,.F.);
#13214=ORIENTED_EDGE('',*,*,#9672,.T.);
#13215=ORIENTED_EDGE('',*,*,#9673,.F.);
#13216=ORIENTED_EDGE('',*,*,#9672,.F.);
#13217=ORIENTED_EDGE('',*,*,#9674,.F.);
#13218=ORIENTED_EDGE('',*,*,#9675,.F.);
#13219=ORIENTED_EDGE('',*,*,#9676,.T.);
#13220=ORIENTED_EDGE('',*,*,#9677,.F.);
#13221=ORIENTED_EDGE('',*,*,#9676,.F.);
#13222=ORIENTED_EDGE('',*,*,#9678,.F.);
#13223=ORIENTED_EDGE('',*,*,#9679,.F.);
#13224=ORIENTED_EDGE('',*,*,#9680,.T.);
#13225=ORIENTED_EDGE('',*,*,#9681,.F.);
#13226=ORIENTED_EDGE('',*,*,#9680,.F.);
#13227=ORIENTED_EDGE('',*,*,#9682,.F.);
#13228=ORIENTED_EDGE('',*,*,#9683,.F.);
#13229=ORIENTED_EDGE('',*,*,#9684,.T.);
#13230=ORIENTED_EDGE('',*,*,#9685,.F.);
#13231=ORIENTED_EDGE('',*,*,#9684,.F.);
#13232=ORIENTED_EDGE('',*,*,#9686,.F.);
#13233=ORIENTED_EDGE('',*,*,#9687,.F.);
#13234=ORIENTED_EDGE('',*,*,#9688,.T.);
#13235=ORIENTED_EDGE('',*,*,#9689,.F.);
#13236=ORIENTED_EDGE('',*,*,#9688,.F.);
#13237=ORIENTED_EDGE('',*,*,#9690,.F.);
#13238=ORIENTED_EDGE('',*,*,#9691,.F.);
#13239=ORIENTED_EDGE('',*,*,#9692,.T.);
#13240=ORIENTED_EDGE('',*,*,#9693,.F.);
#13241=ORIENTED_EDGE('',*,*,#9692,.F.);
#13242=ORIENTED_EDGE('',*,*,#9694,.F.);
#13243=ORIENTED_EDGE('',*,*,#9695,.F.);
#13244=ORIENTED_EDGE('',*,*,#9696,.T.);
#13245=ORIENTED_EDGE('',*,*,#9697,.F.);
#13246=ORIENTED_EDGE('',*,*,#9696,.F.);
#13247=ORIENTED_EDGE('',*,*,#9698,.F.);
#13248=ORIENTED_EDGE('',*,*,#9699,.F.);
#13249=ORIENTED_EDGE('',*,*,#9700,.T.);
#13250=ORIENTED_EDGE('',*,*,#9701,.F.);
#13251=ORIENTED_EDGE('',*,*,#9700,.F.);
#13252=ORIENTED_EDGE('',*,*,#9702,.F.);
#13253=ORIENTED_EDGE('',*,*,#9703,.F.);
#13254=ORIENTED_EDGE('',*,*,#9704,.T.);
#13255=ORIENTED_EDGE('',*,*,#9705,.F.);
#13256=ORIENTED_EDGE('',*,*,#9704,.F.);
#13257=ORIENTED_EDGE('',*,*,#9706,.F.);
#13258=ORIENTED_EDGE('',*,*,#9707,.F.);
#13259=ORIENTED_EDGE('',*,*,#9708,.T.);
#13260=ORIENTED_EDGE('',*,*,#9709,.F.);
#13261=ORIENTED_EDGE('',*,*,#9708,.F.);
#13262=ORIENTED_EDGE('',*,*,#9710,.F.);
#13263=ORIENTED_EDGE('',*,*,#9711,.F.);
#13264=ORIENTED_EDGE('',*,*,#9712,.T.);
#13265=ORIENTED_EDGE('',*,*,#9713,.F.);
#13266=ORIENTED_EDGE('',*,*,#9712,.F.);
#13267=ORIENTED_EDGE('',*,*,#9714,.F.);
#13268=ORIENTED_EDGE('',*,*,#9715,.F.);
#13269=ORIENTED_EDGE('',*,*,#9716,.T.);
#13270=ORIENTED_EDGE('',*,*,#9717,.F.);
#13271=ORIENTED_EDGE('',*,*,#9716,.F.);
#13272=ORIENTED_EDGE('',*,*,#9718,.F.);
#13273=ORIENTED_EDGE('',*,*,#9719,.F.);
#13274=ORIENTED_EDGE('',*,*,#9720,.T.);
#13275=ORIENTED_EDGE('',*,*,#9721,.F.);
#13276=ORIENTED_EDGE('',*,*,#9720,.F.);
#13277=ORIENTED_EDGE('',*,*,#9722,.T.);
#13278=ORIENTED_EDGE('',*,*,#9723,.T.);
#13279=ORIENTED_EDGE('',*,*,#9724,.T.);
#13280=ORIENTED_EDGE('',*,*,#9725,.T.);
#13281=ORIENTED_EDGE('',*,*,#9726,.T.);
#13282=ORIENTED_EDGE('',*,*,#9727,.F.);
#13283=ORIENTED_EDGE('',*,*,#9728,.F.);
#13284=ORIENTED_EDGE('',*,*,#9729,.F.);
#13285=ORIENTED_EDGE('',*,*,#9730,.F.);
#13286=ORIENTED_EDGE('',*,*,#9731,.F.);
#13287=ORIENTED_EDGE('',*,*,#9732,.T.);
#13288=ORIENTED_EDGE('',*,*,#9733,.T.);
#13289=ORIENTED_EDGE('',*,*,#9734,.T.);
#13290=ORIENTED_EDGE('',*,*,#9735,.T.);
#13291=ORIENTED_EDGE('',*,*,#9736,.T.);
#13292=ORIENTED_EDGE('',*,*,#9737,.T.);
#13293=ORIENTED_EDGE('',*,*,#9738,.T.);
#13294=ORIENTED_EDGE('',*,*,#9739,.T.);
#13295=ORIENTED_EDGE('',*,*,#9740,.F.);
#13296=ORIENTED_EDGE('',*,*,#9736,.F.);
#13297=ORIENTED_EDGE('',*,*,#9741,.F.);
#13298=ORIENTED_EDGE('',*,*,#9742,.T.);
#13299=ORIENTED_EDGE('',*,*,#9743,.T.);
#13300=ORIENTED_EDGE('',*,*,#9744,.F.);
#13301=ORIENTED_EDGE('',*,*,#9737,.F.);
#13302=ORIENTED_EDGE('',*,*,#9740,.T.);
#13303=ORIENTED_EDGE('',*,*,#9745,.T.);
#13304=ORIENTED_EDGE('',*,*,#9746,.F.);
#13305=ORIENTED_EDGE('',*,*,#9747,.F.);
#13306=ORIENTED_EDGE('',*,*,#9738,.F.);
#13307=ORIENTED_EDGE('',*,*,#9744,.T.);
#13308=ORIENTED_EDGE('',*,*,#9748,.F.);
#13309=ORIENTED_EDGE('',*,*,#9729,.T.);
#13310=ORIENTED_EDGE('',*,*,#9749,.F.);
#13311=ORIENTED_EDGE('',*,*,#9750,.F.);
#13312=ORIENTED_EDGE('',*,*,#9751,.F.);
#13313=ORIENTED_EDGE('',*,*,#9731,.T.);
#13314=ORIENTED_EDGE('',*,*,#9752,.F.);
#13315=ORIENTED_EDGE('',*,*,#9753,.F.);
#13316=ORIENTED_EDGE('',*,*,#9754,.F.);
#13317=ORIENTED_EDGE('',*,*,#9735,.F.);
#13318=ORIENTED_EDGE('',*,*,#9755,.F.);
#13319=ORIENTED_EDGE('',*,*,#9756,.F.);
#13320=ORIENTED_EDGE('',*,*,#9757,.F.);
#13321=ORIENTED_EDGE('',*,*,#9758,.F.);
#13322=ORIENTED_EDGE('',*,*,#9726,.F.);
#13323=ORIENTED_EDGE('',*,*,#9759,.F.);
#13324=ORIENTED_EDGE('',*,*,#9743,.F.);
#13325=ORIENTED_EDGE('',*,*,#9760,.F.);
#13326=ORIENTED_EDGE('',*,*,#9761,.F.);
#13327=ORIENTED_EDGE('',*,*,#9762,.F.);
#13328=ORIENTED_EDGE('',*,*,#9763,.F.);
#13329=ORIENTED_EDGE('',*,*,#9761,.T.);
#13330=ORIENTED_EDGE('',*,*,#9764,.F.);
#13331=ORIENTED_EDGE('',*,*,#9765,.F.);
#13332=ORIENTED_EDGE('',*,*,#9766,.F.);
#13333=ORIENTED_EDGE('',*,*,#9753,.T.);
#13334=ORIENTED_EDGE('',*,*,#9767,.F.);
#13335=ORIENTED_EDGE('',*,*,#9768,.F.);
#13336=ORIENTED_EDGE('',*,*,#9741,.T.);
#13337=ORIENTED_EDGE('',*,*,#9754,.T.);
#13338=ORIENTED_EDGE('',*,*,#9766,.T.);
#13339=ORIENTED_EDGE('',*,*,#9769,.T.);
#13340=ORIENTED_EDGE('',*,*,#9742,.F.);
#13341=ORIENTED_EDGE('',*,*,#9769,.F.);
#13342=ORIENTED_EDGE('',*,*,#9765,.T.);
#13343=ORIENTED_EDGE('',*,*,#9770,.T.);
#13344=ORIENTED_EDGE('',*,*,#9739,.F.);
#13345=ORIENTED_EDGE('',*,*,#9770,.F.);
#13346=ORIENTED_EDGE('',*,*,#9764,.T.);
#13347=ORIENTED_EDGE('',*,*,#9760,.T.);
#13348=ORIENTED_EDGE('',*,*,#9771,.F.);
#13349=ORIENTED_EDGE('',*,*,#9659,.T.);
#13350=ORIENTED_EDGE('',*,*,#9772,.T.);
#13351=ORIENTED_EDGE('',*,*,#9649,.T.);
#13352=ORIENTED_EDGE('',*,*,#9773,.T.);
#13353=ORIENTED_EDGE('',*,*,#9661,.T.);
#13354=ORIENTED_EDGE('',*,*,#9774,.F.);
#13355=ORIENTED_EDGE('',*,*,#9655,.T.);
#13356=ORIENTED_EDGE('',*,*,#9775,.T.);
#13357=ORIENTED_EDGE('',*,*,#9657,.T.);
#13358=ORIENTED_EDGE('',*,*,#9776,.F.);
#13359=ORIENTED_EDGE('',*,*,#9651,.T.);
#13360=ORIENTED_EDGE('',*,*,#9777,.T.);
#13361=ORIENTED_EDGE('',*,*,#9653,.T.);
#13362=ORIENTED_EDGE('',*,*,#9778,.F.);
#13363=ORIENTED_EDGE('',*,*,#9647,.T.);
#13364=ORIENTED_EDGE('',*,*,#9718,.T.);
#13365=ORIENTED_EDGE('',*,*,#9719,.T.);
#13366=ORIENTED_EDGE('',*,*,#9779,.T.);
#13367=ORIENTED_EDGE('',*,*,#9780,.F.);
#13368=ORIENTED_EDGE('',*,*,#9779,.F.);
#13369=ORIENTED_EDGE('',*,*,#9781,.T.);
#13370=ORIENTED_EDGE('',*,*,#9782,.T.);
#13371=ORIENTED_EDGE('',*,*,#9783,.F.);
#13372=ORIENTED_EDGE('',*,*,#9782,.F.);
#13373=ORIENTED_EDGE('',*,*,#9710,.T.);
#13374=ORIENTED_EDGE('',*,*,#9711,.T.);
#13375=ORIENTED_EDGE('',*,*,#9784,.T.);
#13376=ORIENTED_EDGE('',*,*,#9785,.F.);
#13377=ORIENTED_EDGE('',*,*,#9784,.F.);
#13378=ORIENTED_EDGE('',*,*,#9694,.T.);
#13379=ORIENTED_EDGE('',*,*,#9695,.T.);
#13380=ORIENTED_EDGE('',*,*,#9786,.T.);
#13381=ORIENTED_EDGE('',*,*,#9787,.F.);
#13382=ORIENTED_EDGE('',*,*,#9786,.F.);
#13383=ORIENTED_EDGE('',*,*,#9714,.T.);
#13384=ORIENTED_EDGE('',*,*,#9715,.T.);
#13385=ORIENTED_EDGE('',*,*,#9788,.T.);
#13386=ORIENTED_EDGE('',*,*,#9789,.F.);
#13387=ORIENTED_EDGE('',*,*,#9788,.F.);
#13388=ORIENTED_EDGE('',*,*,#9790,.T.);
#13389=ORIENTED_EDGE('',*,*,#9791,.T.);
#13390=ORIENTED_EDGE('',*,*,#9792,.F.);
#13391=ORIENTED_EDGE('',*,*,#9791,.F.);
#13392=ORIENTED_EDGE('',*,*,#9793,.T.);
#13393=ORIENTED_EDGE('',*,*,#9794,.T.);
#13394=ORIENTED_EDGE('',*,*,#9795,.F.);
#13395=ORIENTED_EDGE('',*,*,#9794,.F.);
#13396=ORIENTED_EDGE('',*,*,#9706,.T.);
#13397=ORIENTED_EDGE('',*,*,#9707,.T.);
#13398=ORIENTED_EDGE('',*,*,#9796,.T.);
#13399=ORIENTED_EDGE('',*,*,#9797,.F.);
#13400=ORIENTED_EDGE('',*,*,#9796,.F.);
#13401=ORIENTED_EDGE('',*,*,#9690,.T.);
#13402=ORIENTED_EDGE('',*,*,#9691,.T.);
#13403=ORIENTED_EDGE('',*,*,#9798,.T.);
#13404=ORIENTED_EDGE('',*,*,#9799,.F.);
#13405=ORIENTED_EDGE('',*,*,#9798,.F.);
#13406=ORIENTED_EDGE('',*,*,#9702,.T.);
#13407=ORIENTED_EDGE('',*,*,#9703,.T.);
#13408=ORIENTED_EDGE('',*,*,#9800,.T.);
#13409=ORIENTED_EDGE('',*,*,#9801,.F.);
#13410=ORIENTED_EDGE('',*,*,#9800,.F.);
#13411=ORIENTED_EDGE('',*,*,#9698,.T.);
#13412=ORIENTED_EDGE('',*,*,#9699,.T.);
#13413=ORIENTED_EDGE('',*,*,#9802,.T.);
#13414=ORIENTED_EDGE('',*,*,#9803,.F.);
#13415=ORIENTED_EDGE('',*,*,#9802,.F.);
#13416=ORIENTED_EDGE('',*,*,#9686,.T.);
#13417=ORIENTED_EDGE('',*,*,#9687,.T.);
#13418=ORIENTED_EDGE('',*,*,#9804,.T.);
#13419=ORIENTED_EDGE('',*,*,#9805,.F.);
#13420=ORIENTED_EDGE('',*,*,#9804,.F.);
#13421=ORIENTED_EDGE('',*,*,#9682,.T.);
#13422=ORIENTED_EDGE('',*,*,#9683,.T.);
#13423=ORIENTED_EDGE('',*,*,#9806,.T.);
#13424=ORIENTED_EDGE('',*,*,#9807,.F.);
#13425=ORIENTED_EDGE('',*,*,#9806,.F.);
#13426=ORIENTED_EDGE('',*,*,#9678,.T.);
#13427=ORIENTED_EDGE('',*,*,#9679,.T.);
#13428=ORIENTED_EDGE('',*,*,#9808,.T.);
#13429=ORIENTED_EDGE('',*,*,#9809,.F.);
#13430=ORIENTED_EDGE('',*,*,#9808,.F.);
#13431=ORIENTED_EDGE('',*,*,#9670,.T.);
#13432=ORIENTED_EDGE('',*,*,#9671,.T.);
#13433=ORIENTED_EDGE('',*,*,#9810,.T.);
#13434=ORIENTED_EDGE('',*,*,#9811,.F.);
#13435=ORIENTED_EDGE('',*,*,#9810,.F.);
#13436=ORIENTED_EDGE('',*,*,#9674,.T.);
#13437=ORIENTED_EDGE('',*,*,#9675,.T.);
#13438=ORIENTED_EDGE('',*,*,#9812,.T.);
#13439=ORIENTED_EDGE('',*,*,#9813,.F.);
#13440=ORIENTED_EDGE('',*,*,#9812,.F.);
#13441=ORIENTED_EDGE('',*,*,#9814,.T.);
#13442=ORIENTED_EDGE('',*,*,#9815,.F.);
#13443=ORIENTED_EDGE('',*,*,#9816,.F.);
#13444=ORIENTED_EDGE('',*,*,#9817,.T.);
#13445=ORIENTED_EDGE('',*,*,#9818,.T.);
#13446=ORIENTED_EDGE('',*,*,#9817,.F.);
#13447=ORIENTED_EDGE('',*,*,#9819,.F.);
#13448=ORIENTED_EDGE('',*,*,#9820,.T.);
#13449=ORIENTED_EDGE('',*,*,#9821,.F.);
#13450=ORIENTED_EDGE('',*,*,#9665,.T.);
#13451=ORIENTED_EDGE('',*,*,#9822,.T.);
#13452=ORIENTED_EDGE('',*,*,#9820,.F.);
#13453=ORIENTED_EDGE('',*,*,#9823,.T.);
#13454=ORIENTED_EDGE('',*,*,#9663,.T.);
#13455=ORIENTED_EDGE('',*,*,#9824,.F.);
#13456=ORIENTED_EDGE('',*,*,#9825,.T.);
#13457=ORIENTED_EDGE('',*,*,#9826,.T.);
#13458=ORIENTED_EDGE('',*,*,#9825,.F.);
#13459=ORIENTED_EDGE('',*,*,#9827,.F.);
#13460=ORIENTED_EDGE('',*,*,#9828,.T.);
#13461=ORIENTED_EDGE('',*,*,#9829,.F.);
#13462=ORIENTED_EDGE('',*,*,#9669,.T.);
#13463=ORIENTED_EDGE('',*,*,#9830,.T.);
#13464=ORIENTED_EDGE('',*,*,#9828,.F.);
#13465=ORIENTED_EDGE('',*,*,#9831,.T.);
#13466=ORIENTED_EDGE('',*,*,#9667,.T.);
#13467=ORIENTED_EDGE('',*,*,#9832,.F.);
#13468=ORIENTED_EDGE('',*,*,#9833,.T.);
#13469=ORIENTED_EDGE('',*,*,#9834,.T.);
#13470=ORIENTED_EDGE('',*,*,#9833,.F.);
#13471=ORIENTED_EDGE('',*,*,#9835,.F.);
#13472=ORIENTED_EDGE('',*,*,#9836,.T.);
#13473=ORIENTED_EDGE('',*,*,#9837,.T.);
#13474=ORIENTED_EDGE('',*,*,#9836,.F.);
#13475=ORIENTED_EDGE('',*,*,#9838,.F.);
#13476=ORIENTED_EDGE('',*,*,#9839,.T.);
#13477=ORIENTED_EDGE('',*,*,#9840,.T.);
#13478=ORIENTED_EDGE('',*,*,#9839,.F.);
#13479=ORIENTED_EDGE('',*,*,#9841,.F.);
#13480=ORIENTED_EDGE('',*,*,#9842,.T.);
#13481=ORIENTED_EDGE('',*,*,#9843,.T.);
#13482=ORIENTED_EDGE('',*,*,#9842,.F.);
#13483=ORIENTED_EDGE('',*,*,#9844,.F.);
#13484=ORIENTED_EDGE('',*,*,#9845,.T.);
#13485=ORIENTED_EDGE('',*,*,#9723,.F.);
#13486=ORIENTED_EDGE('',*,*,#9846,.F.);
#13487=ORIENTED_EDGE('',*,*,#9756,.T.);
#13488=ORIENTED_EDGE('',*,*,#9847,.T.);
#13489=ORIENTED_EDGE('',*,*,#9848,.F.);
#13490=ORIENTED_EDGE('',*,*,#9727,.T.);
#13491=ORIENTED_EDGE('',*,*,#9762,.T.);
#13492=ORIENTED_EDGE('',*,*,#9763,.T.);
#13493=ORIENTED_EDGE('',*,*,#9849,.T.);
#13494=ORIENTED_EDGE('',*,*,#9845,.F.);
#13495=ORIENTED_EDGE('',*,*,#9850,.F.);
#13496=ORIENTED_EDGE('',*,*,#9851,.T.);
#13497=ORIENTED_EDGE('',*,*,#9852,.T.);
#13498=ORIENTED_EDGE('',*,*,#9724,.F.);
#13499=ORIENTED_EDGE('',*,*,#9851,.F.);
#13500=ORIENTED_EDGE('',*,*,#9853,.F.);
#13501=ORIENTED_EDGE('',*,*,#9854,.T.);
#13502=ORIENTED_EDGE('',*,*,#9725,.F.);
#13503=ORIENTED_EDGE('',*,*,#9852,.F.);
#13504=ORIENTED_EDGE('',*,*,#9855,.F.);
#13505=ORIENTED_EDGE('',*,*,#9856,.T.);
#13506=ORIENTED_EDGE('',*,*,#9857,.F.);
#13507=ORIENTED_EDGE('',*,*,#9767,.T.);
#13508=ORIENTED_EDGE('',*,*,#9752,.T.);
#13509=ORIENTED_EDGE('',*,*,#9730,.T.);
#13510=ORIENTED_EDGE('',*,*,#9748,.T.);
#13511=ORIENTED_EDGE('',*,*,#9858,.F.);
#13512=ORIENTED_EDGE('',*,*,#9859,.F.);
#13513=ORIENTED_EDGE('',*,*,#9860,.T.);
#13514=ORIENTED_EDGE('',*,*,#9856,.F.);
#13515=ORIENTED_EDGE('',*,*,#9861,.F.);
#13516=ORIENTED_EDGE('',*,*,#9862,.T.);
#13517=ORIENTED_EDGE('',*,*,#9863,.T.);
#13518=ORIENTED_EDGE('',*,*,#9862,.F.);
#13519=ORIENTED_EDGE('',*,*,#9864,.F.);
#13520=ORIENTED_EDGE('',*,*,#9865,.T.);
#13521=ORIENTED_EDGE('',*,*,#9858,.T.);
#13522=ORIENTED_EDGE('',*,*,#9750,.T.);
#13523=ORIENTED_EDGE('',*,*,#9866,.T.);
#13524=ORIENTED_EDGE('',*,*,#9865,.F.);
#13525=ORIENTED_EDGE('',*,*,#9867,.F.);
#13526=ORIENTED_EDGE('',*,*,#9868,.F.);
#13527=ORIENTED_EDGE('',*,*,#9757,.T.);
#13528=ORIENTED_EDGE('',*,*,#9846,.T.);
#13529=ORIENTED_EDGE('',*,*,#9722,.F.);
#13530=ORIENTED_EDGE('',*,*,#9854,.F.);
#13531=ORIENTED_EDGE('',*,*,#9869,.T.);
#13532=ORIENTED_EDGE('',*,*,#9847,.F.);
#13533=ORIENTED_EDGE('',*,*,#9755,.T.);
#13534=ORIENTED_EDGE('',*,*,#9870,.F.);
#13535=ORIENTED_EDGE('',*,*,#9815,.T.);
#13536=ORIENTED_EDGE('',*,*,#9848,.T.);
#13537=ORIENTED_EDGE('',*,*,#9869,.F.);
#13538=ORIENTED_EDGE('',*,*,#9814,.F.);
#13539=ORIENTED_EDGE('',*,*,#9818,.F.);
#13540=ORIENTED_EDGE('',*,*,#9822,.F.);
#13541=ORIENTED_EDGE('',*,*,#9664,.T.);
#13542=ORIENTED_EDGE('',*,*,#9823,.F.);
#13543=ORIENTED_EDGE('',*,*,#9826,.F.);
#13544=ORIENTED_EDGE('',*,*,#9830,.F.);
#13545=ORIENTED_EDGE('',*,*,#9668,.T.);
#13546=ORIENTED_EDGE('',*,*,#9831,.F.);
#13547=ORIENTED_EDGE('',*,*,#9834,.F.);
#13548=ORIENTED_EDGE('',*,*,#9837,.F.);
#13549=ORIENTED_EDGE('',*,*,#9840,.F.);
#13550=ORIENTED_EDGE('',*,*,#9843,.F.);
#13551=ORIENTED_EDGE('',*,*,#9849,.F.);
#13552=ORIENTED_EDGE('',*,*,#9768,.T.);
#13553=ORIENTED_EDGE('',*,*,#9857,.T.);
#13554=ORIENTED_EDGE('',*,*,#9860,.F.);
#13555=ORIENTED_EDGE('',*,*,#9863,.F.);
#13556=ORIENTED_EDGE('',*,*,#9866,.F.);
#13557=ORIENTED_EDGE('',*,*,#9749,.T.);
#13558=ORIENTED_EDGE('',*,*,#9728,.T.);
#13559=ORIENTED_EDGE('',*,*,#9811,.T.);
#13560=ORIENTED_EDGE('',*,*,#9771,.T.);
#13561=ORIENTED_EDGE('',*,*,#9648,.T.);
#13562=ORIENTED_EDGE('',*,*,#9778,.T.);
#13563=ORIENTED_EDGE('',*,*,#9652,.T.);
#13564=ORIENTED_EDGE('',*,*,#9776,.T.);
#13565=ORIENTED_EDGE('',*,*,#9656,.T.);
#13566=ORIENTED_EDGE('',*,*,#9774,.T.);
#13567=ORIENTED_EDGE('',*,*,#9660,.T.);
#13568=ORIENTED_EDGE('',*,*,#9813,.T.);
#13569=ORIENTED_EDGE('',*,*,#9809,.T.);
#13570=ORIENTED_EDGE('',*,*,#9807,.T.);
#13571=ORIENTED_EDGE('',*,*,#9805,.T.);
#13572=ORIENTED_EDGE('',*,*,#9803,.T.);
#13573=ORIENTED_EDGE('',*,*,#9801,.T.);
#13574=ORIENTED_EDGE('',*,*,#9799,.T.);
#13575=ORIENTED_EDGE('',*,*,#9797,.T.);
#13576=ORIENTED_EDGE('',*,*,#9795,.T.);
#13577=ORIENTED_EDGE('',*,*,#9792,.T.);
#13578=ORIENTED_EDGE('',*,*,#9789,.T.);
#13579=ORIENTED_EDGE('',*,*,#9787,.T.);
#13580=ORIENTED_EDGE('',*,*,#9785,.T.);
#13581=ORIENTED_EDGE('',*,*,#9783,.T.);
#13582=ORIENTED_EDGE('',*,*,#9780,.T.);
#13583=ORIENTED_EDGE('',*,*,#9870,.T.);
#13584=ORIENTED_EDGE('',*,*,#9758,.T.);
#13585=ORIENTED_EDGE('',*,*,#9868,.T.);
#13586=ORIENTED_EDGE('',*,*,#9859,.T.);
#13587=ORIENTED_EDGE('',*,*,#9867,.T.);
#13588=ORIENTED_EDGE('',*,*,#9864,.T.);
#13589=ORIENTED_EDGE('',*,*,#9861,.T.);
#13590=ORIENTED_EDGE('',*,*,#9855,.T.);
#13591=ORIENTED_EDGE('',*,*,#9853,.T.);
#13592=ORIENTED_EDGE('',*,*,#9850,.T.);
#13593=ORIENTED_EDGE('',*,*,#9844,.T.);
#13594=ORIENTED_EDGE('',*,*,#9841,.T.);
#13595=ORIENTED_EDGE('',*,*,#9838,.T.);
#13596=ORIENTED_EDGE('',*,*,#9835,.T.);
#13597=ORIENTED_EDGE('',*,*,#9832,.T.);
#13598=ORIENTED_EDGE('',*,*,#9666,.T.);
#13599=ORIENTED_EDGE('',*,*,#9829,.T.);
#13600=ORIENTED_EDGE('',*,*,#9827,.T.);
#13601=ORIENTED_EDGE('',*,*,#9824,.T.);
#13602=ORIENTED_EDGE('',*,*,#9662,.T.);
#13603=ORIENTED_EDGE('',*,*,#9821,.T.);
#13604=ORIENTED_EDGE('',*,*,#9819,.T.);
#13605=ORIENTED_EDGE('',*,*,#9816,.T.);
#13606=ORIENTED_EDGE('',*,*,#9775,.F.);
#13607=ORIENTED_EDGE('',*,*,#9650,.T.);
#13608=ORIENTED_EDGE('',*,*,#9777,.F.);
#13609=ORIENTED_EDGE('',*,*,#9646,.T.);
#13610=ORIENTED_EDGE('',*,*,#9772,.F.);
#13611=ORIENTED_EDGE('',*,*,#9658,.T.);
#13612=ORIENTED_EDGE('',*,*,#9773,.F.);
#13613=ORIENTED_EDGE('',*,*,#9654,.T.);
#13614=ORIENTED_EDGE('',*,*,#9793,.F.);
#13615=ORIENTED_EDGE('',*,*,#9790,.F.);
#13616=ORIENTED_EDGE('',*,*,#9781,.F.);
#13617=ORIENTED_EDGE('',*,*,#9673,.T.);
#13618=ORIENTED_EDGE('',*,*,#9677,.T.);
#13619=ORIENTED_EDGE('',*,*,#9681,.T.);
#13620=ORIENTED_EDGE('',*,*,#9685,.T.);
#13621=ORIENTED_EDGE('',*,*,#9689,.T.);
#13622=ORIENTED_EDGE('',*,*,#9693,.T.);
#13623=ORIENTED_EDGE('',*,*,#9697,.T.);
#13624=ORIENTED_EDGE('',*,*,#9701,.T.);
#13625=ORIENTED_EDGE('',*,*,#9705,.T.);
#13626=ORIENTED_EDGE('',*,*,#9709,.T.);
#13627=ORIENTED_EDGE('',*,*,#9713,.T.);
#13628=ORIENTED_EDGE('',*,*,#9717,.T.);
#13629=ORIENTED_EDGE('',*,*,#9721,.T.);
#13630=ORIENTED_EDGE('',*,*,#9732,.F.);
#13631=ORIENTED_EDGE('',*,*,#9751,.T.);
#13632=ORIENTED_EDGE('',*,*,#9747,.T.);
#13633=ORIENTED_EDGE('',*,*,#9871,.T.);
#13634=ORIENTED_EDGE('',*,*,#9733,.F.);
#13635=ORIENTED_EDGE('',*,*,#9871,.F.);
#13636=ORIENTED_EDGE('',*,*,#9746,.T.);
#13637=ORIENTED_EDGE('',*,*,#9872,.T.);
#13638=ORIENTED_EDGE('',*,*,#9734,.F.);
#13639=ORIENTED_EDGE('',*,*,#9872,.F.);
#13640=ORIENTED_EDGE('',*,*,#9745,.F.);
#13641=ORIENTED_EDGE('',*,*,#9759,.T.);
#13642=ORIENTED_EDGE('',*,*,#9873,.F.);
#13643=ORIENTED_EDGE('',*,*,#9874,.T.);
#13644=ORIENTED_EDGE('',*,*,#9875,.T.);
#13645=ORIENTED_EDGE('',*,*,#9876,.F.);
#13646=ORIENTED_EDGE('',*,*,#9877,.T.);
#13647=ORIENTED_EDGE('',*,*,#9878,.F.);
#13648=ORIENTED_EDGE('',*,*,#9879,.F.);
#13649=ORIENTED_EDGE('',*,*,#9880,.F.);
#13650=ORIENTED_EDGE('',*,*,#9879,.T.);
#13651=ORIENTED_EDGE('',*,*,#9881,.T.);
#13652=ORIENTED_EDGE('',*,*,#9882,.T.);
#13653=ORIENTED_EDGE('',*,*,#9873,.T.);
#13654=ORIENTED_EDGE('',*,*,#9883,.F.);
#13655=ORIENTED_EDGE('',*,*,#9884,.F.);
#13656=ORIENTED_EDGE('',*,*,#9885,.T.);
#13657=ORIENTED_EDGE('',*,*,#9886,.F.);
#13658=ORIENTED_EDGE('',*,*,#9887,.F.);
#13659=ORIENTED_EDGE('',*,*,#9885,.F.);
#13660=ORIENTED_EDGE('',*,*,#9888,.F.);
#13661=ORIENTED_EDGE('',*,*,#9889,.T.);
#13662=ORIENTED_EDGE('',*,*,#9890,.F.);
#13663=ORIENTED_EDGE('',*,*,#9891,.F.);
#13664=ORIENTED_EDGE('',*,*,#9889,.F.);
#13665=ORIENTED_EDGE('',*,*,#9884,.T.);
#13666=ORIENTED_EDGE('',*,*,#9892,.T.);
#13667=ORIENTED_EDGE('',*,*,#9893,.T.);
#13668=ORIENTED_EDGE('',*,*,#9886,.T.);
#13669=ORIENTED_EDGE('',*,*,#9887,.T.);
#13670=ORIENTED_EDGE('',*,*,#9893,.F.);
#13671=ORIENTED_EDGE('',*,*,#9888,.T.);
#13672=ORIENTED_EDGE('',*,*,#9894,.T.);
#13673=ORIENTED_EDGE('',*,*,#9895,.T.);
#13674=ORIENTED_EDGE('',*,*,#9890,.T.);
#13675=ORIENTED_EDGE('',*,*,#9891,.T.);
#13676=ORIENTED_EDGE('',*,*,#9895,.F.);
#13677=ORIENTED_EDGE('',*,*,#9875,.F.);
#13678=ORIENTED_EDGE('',*,*,#9896,.F.);
#13679=ORIENTED_EDGE('',*,*,#9897,.T.);
#13680=ORIENTED_EDGE('',*,*,#9898,.T.);
#13681=ORIENTED_EDGE('',*,*,#9899,.T.);
#13682=ORIENTED_EDGE('',*,*,#9900,.T.);
#13683=ORIENTED_EDGE('',*,*,#9901,.T.);
#13684=ORIENTED_EDGE('',*,*,#9902,.F.);
#13685=ORIENTED_EDGE('',*,*,#9899,.F.);
#13686=ORIENTED_EDGE('',*,*,#9903,.T.);
#13687=ORIENTED_EDGE('',*,*,#9894,.F.);
#13688=ORIENTED_EDGE('',*,*,#9892,.F.);
#13689=ORIENTED_EDGE('',*,*,#9904,.T.);
#13690=ORIENTED_EDGE('',*,*,#9903,.F.);
#13691=ORIENTED_EDGE('',*,*,#9898,.F.);
#13692=ORIENTED_EDGE('',*,*,#9905,.T.);
#13693=ORIENTED_EDGE('',*,*,#9881,.F.);
#13694=ORIENTED_EDGE('',*,*,#9878,.T.);
#13695=ORIENTED_EDGE('',*,*,#9906,.T.);
#13696=ORIENTED_EDGE('',*,*,#9905,.F.);
#13697=ORIENTED_EDGE('',*,*,#9897,.F.);
#13698=ORIENTED_EDGE('',*,*,#9907,.T.);
#13699=ORIENTED_EDGE('',*,*,#9908,.T.);
#13700=ORIENTED_EDGE('',*,*,#9880,.T.);
#13701=ORIENTED_EDGE('',*,*,#9883,.T.);
#13702=ORIENTED_EDGE('',*,*,#9876,.T.);
#13703=ORIENTED_EDGE('',*,*,#9896,.T.);
#13704=ORIENTED_EDGE('',*,*,#9874,.F.);
#13705=ORIENTED_EDGE('',*,*,#9882,.F.);
#13706=ORIENTED_EDGE('',*,*,#9907,.F.);
#13707=ORIENTED_EDGE('',*,*,#9900,.F.);
#13708=ORIENTED_EDGE('',*,*,#9902,.T.);
#13709=ORIENTED_EDGE('',*,*,#9877,.F.);
#13710=ORIENTED_EDGE('',*,*,#9908,.F.);
#13711=ORIENTED_EDGE('',*,*,#9901,.F.);
#13712=ORIENTED_EDGE('',*,*,#9904,.F.);
#13713=ORIENTED_EDGE('',*,*,#9906,.F.);
#13714=ORIENTED_EDGE('',*,*,#9909,.F.);
#13715=ORIENTED_EDGE('',*,*,#9910,.F.);
#13716=ORIENTED_EDGE('',*,*,#9911,.T.);
#13717=ORIENTED_EDGE('',*,*,#9912,.T.);
#13718=ORIENTED_EDGE('',*,*,#9913,.T.);
#13719=ORIENTED_EDGE('',*,*,#9914,.F.);
#13720=ORIENTED_EDGE('',*,*,#9915,.F.);
#13721=ORIENTED_EDGE('',*,*,#9916,.T.);
#13722=ORIENTED_EDGE('',*,*,#9917,.F.);
#13723=ORIENTED_EDGE('',*,*,#9918,.F.);
#13724=ORIENTED_EDGE('',*,*,#9919,.F.);
#13725=ORIENTED_EDGE('',*,*,#9920,.F.);
#13726=ORIENTED_EDGE('',*,*,#9921,.F.);
#13727=ORIENTED_EDGE('',*,*,#9922,.F.);
#13728=ORIENTED_EDGE('',*,*,#9923,.F.);
#13729=ORIENTED_EDGE('',*,*,#9924,.F.);
#13730=ORIENTED_EDGE('',*,*,#9925,.F.);
#13731=ORIENTED_EDGE('',*,*,#9926,.F.);
#13732=ORIENTED_EDGE('',*,*,#9927,.F.);
#13733=ORIENTED_EDGE('',*,*,#9928,.F.);
#13734=ORIENTED_EDGE('',*,*,#9929,.F.);
#13735=ORIENTED_EDGE('',*,*,#9930,.F.);
#13736=ORIENTED_EDGE('',*,*,#9931,.F.);
#13737=ORIENTED_EDGE('',*,*,#9932,.F.);
#13738=ORIENTED_EDGE('',*,*,#9933,.T.);
#13739=ORIENTED_EDGE('',*,*,#9924,.T.);
#13740=ORIENTED_EDGE('',*,*,#9934,.T.);
#13741=ORIENTED_EDGE('',*,*,#9935,.T.);
#13742=ORIENTED_EDGE('',*,*,#9936,.F.);
#13743=ORIENTED_EDGE('',*,*,#9922,.T.);
#13744=ORIENTED_EDGE('',*,*,#9937,.T.);
#13745=ORIENTED_EDGE('',*,*,#9920,.T.);
#13746=ORIENTED_EDGE('',*,*,#9938,.T.);
#13747=ORIENTED_EDGE('',*,*,#9928,.T.);
#13748=ORIENTED_EDGE('',*,*,#9939,.T.);
#13749=ORIENTED_EDGE('',*,*,#9940,.T.);
#13750=ORIENTED_EDGE('',*,*,#9941,.T.);
#13751=ORIENTED_EDGE('',*,*,#9932,.T.);
#13752=ORIENTED_EDGE('',*,*,#9942,.F.);
#13753=ORIENTED_EDGE('',*,*,#9926,.T.);
#13754=ORIENTED_EDGE('',*,*,#9943,.F.);
#13755=ORIENTED_EDGE('',*,*,#9944,.F.);
#13756=ORIENTED_EDGE('',*,*,#9930,.T.);
#13757=ORIENTED_EDGE('',*,*,#9945,.F.);
#13758=ORIENTED_EDGE('',*,*,#9946,.F.);
#13759=ORIENTED_EDGE('',*,*,#9947,.F.);
#13760=ORIENTED_EDGE('',*,*,#9948,.F.);
#13761=ORIENTED_EDGE('',*,*,#9949,.F.);
#13762=ORIENTED_EDGE('',*,*,#9950,.F.);
#13763=ORIENTED_EDGE('',*,*,#9951,.F.);
#13764=ORIENTED_EDGE('',*,*,#9914,.T.);
#13765=ORIENTED_EDGE('',*,*,#9952,.T.);
#13766=ORIENTED_EDGE('',*,*,#9953,.T.);
#13767=ORIENTED_EDGE('',*,*,#9912,.F.);
#13768=ORIENTED_EDGE('',*,*,#9954,.T.);
#13769=ORIENTED_EDGE('',*,*,#9955,.T.);
#13770=ORIENTED_EDGE('',*,*,#9956,.T.);
#13771=ORIENTED_EDGE('',*,*,#9957,.T.);
#13772=ORIENTED_EDGE('',*,*,#9958,.T.);
#13773=ORIENTED_EDGE('',*,*,#9959,.T.);
#13774=ORIENTED_EDGE('',*,*,#9960,.T.);
#13775=ORIENTED_EDGE('',*,*,#9918,.T.);
#13776=ORIENTED_EDGE('',*,*,#9941,.F.);
#13777=ORIENTED_EDGE('',*,*,#9925,.T.);
#13778=ORIENTED_EDGE('',*,*,#9938,.F.);
#13779=ORIENTED_EDGE('',*,*,#9961,.F.);
#13780=ORIENTED_EDGE('',*,*,#9934,.F.);
#13781=ORIENTED_EDGE('',*,*,#9923,.T.);
#13782=ORIENTED_EDGE('',*,*,#9936,.T.);
#13783=ORIENTED_EDGE('',*,*,#9919,.T.);
#13784=ORIENTED_EDGE('',*,*,#9960,.F.);
#13785=ORIENTED_EDGE('',*,*,#9962,.T.);
#13786=ORIENTED_EDGE('',*,*,#9945,.T.);
#13787=ORIENTED_EDGE('',*,*,#9929,.T.);
#13788=ORIENTED_EDGE('',*,*,#9946,.T.);
#13789=ORIENTED_EDGE('',*,*,#9962,.F.);
#13790=ORIENTED_EDGE('',*,*,#9959,.F.);
#13791=ORIENTED_EDGE('',*,*,#9963,.T.);
#13792=ORIENTED_EDGE('',*,*,#9947,.T.);
#13793=ORIENTED_EDGE('',*,*,#9963,.F.);
#13794=ORIENTED_EDGE('',*,*,#9958,.F.);
#13795=ORIENTED_EDGE('',*,*,#9964,.T.);
#13796=ORIENTED_EDGE('',*,*,#9948,.T.);
#13797=ORIENTED_EDGE('',*,*,#9964,.F.);
#13798=ORIENTED_EDGE('',*,*,#9957,.F.);
#13799=ORIENTED_EDGE('',*,*,#9965,.T.);
#13800=ORIENTED_EDGE('',*,*,#9949,.T.);
#13801=ORIENTED_EDGE('',*,*,#9965,.F.);
#13802=ORIENTED_EDGE('',*,*,#9956,.F.);
#13803=ORIENTED_EDGE('',*,*,#9966,.T.);
#13804=ORIENTED_EDGE('',*,*,#9950,.T.);
#13805=ORIENTED_EDGE('',*,*,#9966,.F.);
#13806=ORIENTED_EDGE('',*,*,#9955,.F.);
#13807=ORIENTED_EDGE('',*,*,#9967,.T.);
#13808=ORIENTED_EDGE('',*,*,#9968,.T.);
#13809=ORIENTED_EDGE('',*,*,#9915,.T.);
#13810=ORIENTED_EDGE('',*,*,#9951,.T.);
#13811=ORIENTED_EDGE('',*,*,#9967,.F.);
#13812=ORIENTED_EDGE('',*,*,#9954,.F.);
#13813=ORIENTED_EDGE('',*,*,#9911,.F.);
#13814=ORIENTED_EDGE('',*,*,#9969,.T.);
#13815=ORIENTED_EDGE('',*,*,#9916,.F.);
#13816=ORIENTED_EDGE('',*,*,#9968,.F.);
#13817=ORIENTED_EDGE('',*,*,#9910,.T.);
#13818=ORIENTED_EDGE('',*,*,#9939,.F.);
#13819=ORIENTED_EDGE('',*,*,#9927,.T.);
#13820=ORIENTED_EDGE('',*,*,#9942,.T.);
#13821=ORIENTED_EDGE('',*,*,#9931,.T.);
#13822=ORIENTED_EDGE('',*,*,#9944,.T.);
#13823=ORIENTED_EDGE('',*,*,#9970,.F.);
#13824=ORIENTED_EDGE('',*,*,#9952,.F.);
#13825=ORIENTED_EDGE('',*,*,#9917,.T.);
#13826=ORIENTED_EDGE('',*,*,#9937,.F.);
#13827=ORIENTED_EDGE('',*,*,#9921,.T.);
#13828=ORIENTED_EDGE('',*,*,#9933,.F.);
#13829=ORIENTED_EDGE('',*,*,#9971,.T.);
#13830=ORIENTED_EDGE('',*,*,#9935,.F.);
#13831=ORIENTED_EDGE('',*,*,#9961,.T.);
#13832=ORIENTED_EDGE('',*,*,#9940,.F.);
#13833=ORIENTED_EDGE('',*,*,#9971,.F.);
#13834=ORIENTED_EDGE('',*,*,#9943,.T.);
#13835=ORIENTED_EDGE('',*,*,#9913,.F.);
#13836=ORIENTED_EDGE('',*,*,#9969,.F.);
#13837=ORIENTED_EDGE('',*,*,#9909,.T.);
#13838=ORIENTED_EDGE('',*,*,#9953,.F.);
#13839=ORIENTED_EDGE('',*,*,#9970,.T.);
#13840=ORIENTED_EDGE('',*,*,#9972,.T.);
#13841=ORIENTED_EDGE('',*,*,#9973,.F.);
#13842=ORIENTED_EDGE('',*,*,#9974,.T.);
#13843=ORIENTED_EDGE('',*,*,#9975,.T.);
#13844=ORIENTED_EDGE('',*,*,#9976,.T.);
#13845=ORIENTED_EDGE('',*,*,#9977,.F.);
#13846=ORIENTED_EDGE('',*,*,#9972,.F.);
#13847=ORIENTED_EDGE('',*,*,#9978,.T.);
#13848=ORIENTED_EDGE('',*,*,#9979,.T.);
#13849=ORIENTED_EDGE('',*,*,#9980,.F.);
#13850=ORIENTED_EDGE('',*,*,#9976,.F.);
#13851=ORIENTED_EDGE('',*,*,#9981,.T.);
#13852=ORIENTED_EDGE('',*,*,#9982,.T.);
#13853=ORIENTED_EDGE('',*,*,#9983,.F.);
#13854=ORIENTED_EDGE('',*,*,#9979,.F.);
#13855=ORIENTED_EDGE('',*,*,#9984,.T.);
#13856=ORIENTED_EDGE('',*,*,#9985,.T.);
#13857=ORIENTED_EDGE('',*,*,#9986,.F.);
#13858=ORIENTED_EDGE('',*,*,#9982,.F.);
#13859=ORIENTED_EDGE('',*,*,#9987,.T.);
#13860=ORIENTED_EDGE('',*,*,#9988,.T.);
#13861=ORIENTED_EDGE('',*,*,#9989,.F.);
#13862=ORIENTED_EDGE('',*,*,#9985,.F.);
#13863=ORIENTED_EDGE('',*,*,#9990,.T.);
#13864=ORIENTED_EDGE('',*,*,#9991,.T.);
#13865=ORIENTED_EDGE('',*,*,#9992,.F.);
#13866=ORIENTED_EDGE('',*,*,#9988,.F.);
#13867=ORIENTED_EDGE('',*,*,#9993,.T.);
#13868=ORIENTED_EDGE('',*,*,#9994,.T.);
#13869=ORIENTED_EDGE('',*,*,#9995,.F.);
#13870=ORIENTED_EDGE('',*,*,#9991,.F.);
#13871=ORIENTED_EDGE('',*,*,#9996,.T.);
#13872=ORIENTED_EDGE('',*,*,#9997,.T.);
#13873=ORIENTED_EDGE('',*,*,#9998,.F.);
#13874=ORIENTED_EDGE('',*,*,#9994,.F.);
#13875=ORIENTED_EDGE('',*,*,#9999,.T.);
#13876=ORIENTED_EDGE('',*,*,#10000,.T.);
#13877=ORIENTED_EDGE('',*,*,#10001,.F.);
#13878=ORIENTED_EDGE('',*,*,#9997,.F.);
#13879=ORIENTED_EDGE('',*,*,#10002,.T.);
#13880=ORIENTED_EDGE('',*,*,#10003,.T.);
#13881=ORIENTED_EDGE('',*,*,#10004,.F.);
#13882=ORIENTED_EDGE('',*,*,#10000,.F.);
#13883=ORIENTED_EDGE('',*,*,#10005,.T.);
#13884=ORIENTED_EDGE('',*,*,#10006,.T.);
#13885=ORIENTED_EDGE('',*,*,#10007,.F.);
#13886=ORIENTED_EDGE('',*,*,#10003,.F.);
#13887=ORIENTED_EDGE('',*,*,#10008,.T.);
#13888=ORIENTED_EDGE('',*,*,#10009,.T.);
#13889=ORIENTED_EDGE('',*,*,#10010,.F.);
#13890=ORIENTED_EDGE('',*,*,#10006,.F.);
#13891=ORIENTED_EDGE('',*,*,#10011,.T.);
#13892=ORIENTED_EDGE('',*,*,#10012,.T.);
#13893=ORIENTED_EDGE('',*,*,#10013,.F.);
#13894=ORIENTED_EDGE('',*,*,#10009,.F.);
#13895=ORIENTED_EDGE('',*,*,#10014,.T.);
#13896=ORIENTED_EDGE('',*,*,#10015,.T.);
#13897=ORIENTED_EDGE('',*,*,#10016,.F.);
#13898=ORIENTED_EDGE('',*,*,#10012,.F.);
#13899=ORIENTED_EDGE('',*,*,#10017,.T.);
#13900=ORIENTED_EDGE('',*,*,#10018,.T.);
#13901=ORIENTED_EDGE('',*,*,#10019,.F.);
#13902=ORIENTED_EDGE('',*,*,#10015,.F.);
#13903=ORIENTED_EDGE('',*,*,#10020,.T.);
#13904=ORIENTED_EDGE('',*,*,#10021,.T.);
#13905=ORIENTED_EDGE('',*,*,#10022,.F.);
#13906=ORIENTED_EDGE('',*,*,#10018,.F.);
#13907=ORIENTED_EDGE('',*,*,#10023,.T.);
#13908=ORIENTED_EDGE('',*,*,#10024,.T.);
#13909=ORIENTED_EDGE('',*,*,#10025,.F.);
#13910=ORIENTED_EDGE('',*,*,#10021,.F.);
#13911=ORIENTED_EDGE('',*,*,#10026,.T.);
#13912=ORIENTED_EDGE('',*,*,#10027,.F.);
#13913=ORIENTED_EDGE('',*,*,#10028,.T.);
#13914=ORIENTED_EDGE('',*,*,#10029,.T.);
#13915=ORIENTED_EDGE('',*,*,#10030,.F.);
#13916=ORIENTED_EDGE('',*,*,#10031,.F.);
#13917=ORIENTED_EDGE('',*,*,#10032,.T.);
#13918=ORIENTED_EDGE('',*,*,#10033,.T.);
#13919=ORIENTED_EDGE('',*,*,#10034,.F.);
#13920=ORIENTED_EDGE('',*,*,#10035,.F.);
#13921=ORIENTED_EDGE('',*,*,#10036,.T.);
#13922=ORIENTED_EDGE('',*,*,#10037,.T.);
#13923=ORIENTED_EDGE('',*,*,#10038,.F.);
#13924=ORIENTED_EDGE('',*,*,#10039,.F.);
#13925=ORIENTED_EDGE('',*,*,#10040,.T.);
#13926=ORIENTED_EDGE('',*,*,#10041,.T.);
#13927=ORIENTED_EDGE('',*,*,#10036,.F.);
#13928=ORIENTED_EDGE('',*,*,#10042,.F.);
#13929=ORIENTED_EDGE('',*,*,#10043,.T.);
#13930=ORIENTED_EDGE('',*,*,#10044,.T.);
#13931=ORIENTED_EDGE('',*,*,#10040,.F.);
#13932=ORIENTED_EDGE('',*,*,#10045,.F.);
#13933=ORIENTED_EDGE('',*,*,#10046,.T.);
#13934=ORIENTED_EDGE('',*,*,#10047,.T.);
#13935=ORIENTED_EDGE('',*,*,#10043,.F.);
#13936=ORIENTED_EDGE('',*,*,#10048,.F.);
#13937=ORIENTED_EDGE('',*,*,#10049,.T.);
#13938=ORIENTED_EDGE('',*,*,#10050,.T.);
#13939=ORIENTED_EDGE('',*,*,#10046,.F.);
#13940=ORIENTED_EDGE('',*,*,#10051,.F.);
#13941=ORIENTED_EDGE('',*,*,#10052,.T.);
#13942=ORIENTED_EDGE('',*,*,#10053,.T.);
#13943=ORIENTED_EDGE('',*,*,#10049,.F.);
#13944=ORIENTED_EDGE('',*,*,#10054,.F.);
#13945=ORIENTED_EDGE('',*,*,#10055,.T.);
#13946=ORIENTED_EDGE('',*,*,#10056,.T.);
#13947=ORIENTED_EDGE('',*,*,#10052,.F.);
#13948=ORIENTED_EDGE('',*,*,#10057,.F.);
#13949=ORIENTED_EDGE('',*,*,#10058,.T.);
#13950=ORIENTED_EDGE('',*,*,#10059,.T.);
#13951=ORIENTED_EDGE('',*,*,#10055,.F.);
#13952=ORIENTED_EDGE('',*,*,#10060,.F.);
#13953=ORIENTED_EDGE('',*,*,#10061,.T.);
#13954=ORIENTED_EDGE('',*,*,#10062,.T.);
#13955=ORIENTED_EDGE('',*,*,#10058,.F.);
#13956=ORIENTED_EDGE('',*,*,#10063,.F.);
#13957=ORIENTED_EDGE('',*,*,#10064,.T.);
#13958=ORIENTED_EDGE('',*,*,#10065,.T.);
#13959=ORIENTED_EDGE('',*,*,#10061,.F.);
#13960=ORIENTED_EDGE('',*,*,#10066,.F.);
#13961=ORIENTED_EDGE('',*,*,#10067,.T.);
#13962=ORIENTED_EDGE('',*,*,#10068,.T.);
#13963=ORIENTED_EDGE('',*,*,#10064,.F.);
#13964=ORIENTED_EDGE('',*,*,#10069,.F.);
#13965=ORIENTED_EDGE('',*,*,#10070,.T.);
#13966=ORIENTED_EDGE('',*,*,#10071,.T.);
#13967=ORIENTED_EDGE('',*,*,#10067,.F.);
#13968=ORIENTED_EDGE('',*,*,#10072,.F.);
#13969=ORIENTED_EDGE('',*,*,#10073,.T.);
#13970=ORIENTED_EDGE('',*,*,#10074,.T.);
#13971=ORIENTED_EDGE('',*,*,#10070,.F.);
#13972=ORIENTED_EDGE('',*,*,#10075,.F.);
#13973=ORIENTED_EDGE('',*,*,#10076,.T.);
#13974=ORIENTED_EDGE('',*,*,#10077,.T.);
#13975=ORIENTED_EDGE('',*,*,#10073,.F.);
#13976=ORIENTED_EDGE('',*,*,#10078,.F.);
#13977=ORIENTED_EDGE('',*,*,#10079,.T.);
#13978=ORIENTED_EDGE('',*,*,#10080,.T.);
#13979=ORIENTED_EDGE('',*,*,#10076,.F.);
#13980=ORIENTED_EDGE('',*,*,#10081,.F.);
#13981=ORIENTED_EDGE('',*,*,#10082,.T.);
#13982=ORIENTED_EDGE('',*,*,#10083,.T.);
#13983=ORIENTED_EDGE('',*,*,#10079,.F.);
#13984=ORIENTED_EDGE('',*,*,#10084,.F.);
#13985=ORIENTED_EDGE('',*,*,#10085,.T.);
#13986=ORIENTED_EDGE('',*,*,#10086,.T.);
#13987=ORIENTED_EDGE('',*,*,#10082,.F.);
#13988=ORIENTED_EDGE('',*,*,#10087,.F.);
#13989=ORIENTED_EDGE('',*,*,#10088,.T.);
#13990=ORIENTED_EDGE('',*,*,#10089,.T.);
#13991=ORIENTED_EDGE('',*,*,#10085,.F.);
#13992=ORIENTED_EDGE('',*,*,#10090,.F.);
#13993=ORIENTED_EDGE('',*,*,#10091,.T.);
#13994=ORIENTED_EDGE('',*,*,#10092,.T.);
#13995=ORIENTED_EDGE('',*,*,#10088,.F.);
#13996=ORIENTED_EDGE('',*,*,#10093,.F.);
#13997=ORIENTED_EDGE('',*,*,#10094,.F.);
#13998=ORIENTED_EDGE('',*,*,#10095,.F.);
#13999=ORIENTED_EDGE('',*,*,#10096,.F.);
#14000=ORIENTED_EDGE('',*,*,#10097,.T.);
#14001=ORIENTED_EDGE('',*,*,#10098,.F.);
#14002=ORIENTED_EDGE('',*,*,#10099,.F.);
#14003=ORIENTED_EDGE('',*,*,#10100,.T.);
#14004=ORIENTED_EDGE('',*,*,#10101,.T.);
#14005=ORIENTED_EDGE('',*,*,#10102,.F.);
#14006=ORIENTED_EDGE('',*,*,#10103,.F.);
#14007=ORIENTED_EDGE('',*,*,#10098,.T.);
#14008=ORIENTED_EDGE('',*,*,#10104,.T.);
#14009=ORIENTED_EDGE('',*,*,#10105,.F.);
#14010=ORIENTED_EDGE('',*,*,#10106,.F.);
#14011=ORIENTED_EDGE('',*,*,#10102,.T.);
#14012=ORIENTED_EDGE('',*,*,#10107,.T.);
#14013=ORIENTED_EDGE('',*,*,#10108,.F.);
#14014=ORIENTED_EDGE('',*,*,#10109,.T.);
#14015=ORIENTED_EDGE('',*,*,#10110,.T.);
#14016=ORIENTED_EDGE('',*,*,#10111,.F.);
#14017=ORIENTED_EDGE('',*,*,#10112,.F.);
#14018=ORIENTED_EDGE('',*,*,#10113,.T.);
#14019=ORIENTED_EDGE('',*,*,#10108,.T.);
#14020=ORIENTED_EDGE('',*,*,#10114,.F.);
#14021=ORIENTED_EDGE('',*,*,#10115,.F.);
#14022=ORIENTED_EDGE('',*,*,#10116,.T.);
#14023=ORIENTED_EDGE('',*,*,#10112,.T.);
#14024=ORIENTED_EDGE('',*,*,#10117,.F.);
#14025=ORIENTED_EDGE('',*,*,#10118,.F.);
#14026=ORIENTED_EDGE('',*,*,#10119,.T.);
#14027=ORIENTED_EDGE('',*,*,#10115,.T.);
#14028=ORIENTED_EDGE('',*,*,#10120,.F.);
#14029=ORIENTED_EDGE('',*,*,#10121,.F.);
#14030=ORIENTED_EDGE('',*,*,#10122,.T.);
#14031=ORIENTED_EDGE('',*,*,#10118,.T.);
#14032=ORIENTED_EDGE('',*,*,#10123,.F.);
#14033=ORIENTED_EDGE('',*,*,#10124,.F.);
#14034=ORIENTED_EDGE('',*,*,#10125,.T.);
#14035=ORIENTED_EDGE('',*,*,#10121,.T.);
#14036=ORIENTED_EDGE('',*,*,#10126,.F.);
#14037=ORIENTED_EDGE('',*,*,#10127,.F.);
#14038=ORIENTED_EDGE('',*,*,#10128,.T.);
#14039=ORIENTED_EDGE('',*,*,#10124,.T.);
#14040=ORIENTED_EDGE('',*,*,#10129,.F.);
#14041=ORIENTED_EDGE('',*,*,#10130,.F.);
#14042=ORIENTED_EDGE('',*,*,#10131,.T.);
#14043=ORIENTED_EDGE('',*,*,#10127,.T.);
#14044=ORIENTED_EDGE('',*,*,#10132,.F.);
#14045=ORIENTED_EDGE('',*,*,#10133,.T.);
#14046=ORIENTED_EDGE('',*,*,#10134,.T.);
#14047=ORIENTED_EDGE('',*,*,#10135,.T.);
#14048=ORIENTED_EDGE('',*,*,#10136,.T.);
#14049=ORIENTED_EDGE('',*,*,#10137,.T.);
#14050=ORIENTED_EDGE('',*,*,#10138,.T.);
#14051=ORIENTED_EDGE('',*,*,#10133,.F.);
#14052=ORIENTED_EDGE('',*,*,#10139,.T.);
#14053=ORIENTED_EDGE('',*,*,#10140,.T.);
#14054=ORIENTED_EDGE('',*,*,#10141,.T.);
#14055=ORIENTED_EDGE('',*,*,#10137,.F.);
#14056=ORIENTED_EDGE('',*,*,#10142,.T.);
#14057=ORIENTED_EDGE('',*,*,#10143,.F.);
#14058=ORIENTED_EDGE('',*,*,#10144,.T.);
#14059=ORIENTED_EDGE('',*,*,#10145,.F.);
#14060=ORIENTED_EDGE('',*,*,#10146,.T.);
#14061=ORIENTED_EDGE('',*,*,#10143,.T.);
#14062=ORIENTED_EDGE('',*,*,#10147,.T.);
#14063=ORIENTED_EDGE('',*,*,#10140,.F.);
#14064=ORIENTED_EDGE('',*,*,#10148,.T.);
#14065=ORIENTED_EDGE('',*,*,#10149,.T.);
#14066=ORIENTED_EDGE('',*,*,#10150,.F.);
#14067=ORIENTED_EDGE('',*,*,#10151,.F.);
#14068=ORIENTED_EDGE('',*,*,#10152,.F.);
#14069=ORIENTED_EDGE('',*,*,#10153,.T.);
#14070=ORIENTED_EDGE('',*,*,#10154,.T.);
#14071=ORIENTED_EDGE('',*,*,#10151,.T.);
#14072=ORIENTED_EDGE('',*,*,#10155,.F.);
#14073=ORIENTED_EDGE('',*,*,#10156,.T.);
#14074=ORIENTED_EDGE('',*,*,#10155,.T.);
#14075=ORIENTED_EDGE('',*,*,#10150,.T.);
#14076=ORIENTED_EDGE('',*,*,#10157,.T.);
#14077=ORIENTED_EDGE('',*,*,#10158,.T.);
#14078=ORIENTED_EDGE('',*,*,#10159,.T.);
#14079=ORIENTED_EDGE('',*,*,#10160,.T.);
#14080=ORIENTED_EDGE('',*,*,#10161,.T.);
#14081=ORIENTED_EDGE('',*,*,#10152,.T.);
#14082=ORIENTED_EDGE('',*,*,#10154,.F.);
#14083=ORIENTED_EDGE('',*,*,#10162,.F.);
#14084=ORIENTED_EDGE('',*,*,#10163,.F.);
#14085=ORIENTED_EDGE('',*,*,#10164,.F.);
#14086=ORIENTED_EDGE('',*,*,#10165,.F.);
#14087=ORIENTED_EDGE('',*,*,#10166,.T.);
#14088=ORIENTED_EDGE('',*,*,#10167,.T.);
#14089=ORIENTED_EDGE('',*,*,#10168,.T.);
#14090=ORIENTED_EDGE('',*,*,#10164,.T.);
#14091=ORIENTED_EDGE('',*,*,#10169,.F.);
#14092=ORIENTED_EDGE('',*,*,#10170,.T.);
#14093=ORIENTED_EDGE('',*,*,#10169,.T.);
#14094=ORIENTED_EDGE('',*,*,#10163,.T.);
#14095=ORIENTED_EDGE('',*,*,#10171,.F.);
#14096=ORIENTED_EDGE('',*,*,#10172,.T.);
#14097=ORIENTED_EDGE('',*,*,#10171,.T.);
#14098=ORIENTED_EDGE('',*,*,#10162,.T.);
#14099=ORIENTED_EDGE('',*,*,#10173,.T.);
#14100=ORIENTED_EDGE('',*,*,#10174,.T.);
#14101=ORIENTED_EDGE('',*,*,#10175,.F.);
#14102=ORIENTED_EDGE('',*,*,#10176,.F.);
#14103=ORIENTED_EDGE('',*,*,#10177,.F.);
#14104=ORIENTED_EDGE('',*,*,#10178,.F.);
#14105=ORIENTED_EDGE('',*,*,#10179,.T.);
#14106=ORIENTED_EDGE('',*,*,#10180,.T.);
#14107=ORIENTED_EDGE('',*,*,#10181,.T.);
#14108=ORIENTED_EDGE('',*,*,#10177,.T.);
#14109=ORIENTED_EDGE('',*,*,#10182,.F.);
#14110=ORIENTED_EDGE('',*,*,#10183,.T.);
#14111=ORIENTED_EDGE('',*,*,#10182,.T.);
#14112=ORIENTED_EDGE('',*,*,#10176,.T.);
#14113=ORIENTED_EDGE('',*,*,#10184,.F.);
#14114=ORIENTED_EDGE('',*,*,#10185,.T.);
#14115=ORIENTED_EDGE('',*,*,#10184,.T.);
#14116=ORIENTED_EDGE('',*,*,#10175,.T.);
#14117=ORIENTED_EDGE('',*,*,#10186,.T.);
#14118=ORIENTED_EDGE('',*,*,#10187,.T.);
#14119=ORIENTED_EDGE('',*,*,#10188,.F.);
#14120=ORIENTED_EDGE('',*,*,#10189,.F.);
#14121=ORIENTED_EDGE('',*,*,#10190,.F.);
#14122=ORIENTED_EDGE('',*,*,#10191,.F.);
#14123=ORIENTED_EDGE('',*,*,#10192,.F.);
#14124=ORIENTED_EDGE('',*,*,#10193,.T.);
#14125=ORIENTED_EDGE('',*,*,#10194,.T.);
#14126=ORIENTED_EDGE('',*,*,#10195,.T.);
#14127=ORIENTED_EDGE('',*,*,#10190,.T.);
#14128=ORIENTED_EDGE('',*,*,#10196,.F.);
#14129=ORIENTED_EDGE('',*,*,#10197,.T.);
#14130=ORIENTED_EDGE('',*,*,#10198,.T.);
#14131=ORIENTED_EDGE('',*,*,#10196,.T.);
#14132=ORIENTED_EDGE('',*,*,#10189,.T.);
#14133=ORIENTED_EDGE('',*,*,#10199,.F.);
#14134=ORIENTED_EDGE('',*,*,#10200,.T.);
#14135=ORIENTED_EDGE('',*,*,#10199,.T.);
#14136=ORIENTED_EDGE('',*,*,#10188,.T.);
#14137=ORIENTED_EDGE('',*,*,#10201,.T.);
#14138=ORIENTED_EDGE('',*,*,#10202,.T.);
#14139=ORIENTED_EDGE('',*,*,#10158,.F.);
#14140=ORIENTED_EDGE('',*,*,#10203,.F.);
#14141=ORIENTED_EDGE('',*,*,#10167,.F.);
#14142=ORIENTED_EDGE('',*,*,#10204,.T.);
#14143=ORIENTED_EDGE('',*,*,#10157,.F.);
#14144=ORIENTED_EDGE('',*,*,#10205,.F.);
#14145=ORIENTED_EDGE('',*,*,#10168,.F.);
#14146=ORIENTED_EDGE('',*,*,#10203,.T.);
#14147=ORIENTED_EDGE('',*,*,#10206,.F.);
#14148=ORIENTED_EDGE('',*,*,#10207,.T.);
#14149=ORIENTED_EDGE('',*,*,#10191,.T.);
#14150=ORIENTED_EDGE('',*,*,#10208,.T.);
#14151=ORIENTED_EDGE('',*,*,#10178,.T.);
#14152=ORIENTED_EDGE('',*,*,#10209,.T.);
#14153=ORIENTED_EDGE('',*,*,#10165,.T.);
#14154=ORIENTED_EDGE('',*,*,#10205,.T.);
#14155=ORIENTED_EDGE('',*,*,#10149,.F.);
#14156=ORIENTED_EDGE('',*,*,#10210,.T.);
#14157=ORIENTED_EDGE('',*,*,#10192,.T.);
#14158=ORIENTED_EDGE('',*,*,#10207,.F.);
#14159=ORIENTED_EDGE('',*,*,#10206,.T.);
#14160=ORIENTED_EDGE('',*,*,#10211,.F.);
#14161=ORIENTED_EDGE('',*,*,#10100,.F.);
#14162=ORIENTED_EDGE('',*,*,#10212,.F.);
#14163=ORIENTED_EDGE('',*,*,#10135,.F.);
#14164=ORIENTED_EDGE('',*,*,#10213,.F.);
#14165=ORIENTED_EDGE('',*,*,#10214,.T.);
#14166=ORIENTED_EDGE('',*,*,#10215,.T.);
#14167=ORIENTED_EDGE('',*,*,#10214,.F.);
#14168=ORIENTED_EDGE('',*,*,#10216,.F.);
#14169=ORIENTED_EDGE('',*,*,#10217,.T.);
#14170=ORIENTED_EDGE('',*,*,#10213,.T.);
#14171=ORIENTED_EDGE('',*,*,#10217,.F.);
#14172=ORIENTED_EDGE('',*,*,#10170,.F.);
#14173=ORIENTED_EDGE('',*,*,#10172,.F.);
#14174=ORIENTED_EDGE('',*,*,#10218,.F.);
#14175=ORIENTED_EDGE('',*,*,#10179,.F.);
#14176=ORIENTED_EDGE('',*,*,#10183,.F.);
#14177=ORIENTED_EDGE('',*,*,#10185,.F.);
#14178=ORIENTED_EDGE('',*,*,#10219,.F.);
#14179=ORIENTED_EDGE('',*,*,#10193,.F.);
#14180=ORIENTED_EDGE('',*,*,#10198,.F.);
#14181=ORIENTED_EDGE('',*,*,#10220,.T.);
#14182=ORIENTED_EDGE('',*,*,#10216,.T.);
#14183=ORIENTED_EDGE('',*,*,#10220,.F.);
#14184=ORIENTED_EDGE('',*,*,#10197,.F.);
#14185=ORIENTED_EDGE('',*,*,#10200,.F.);
#14186=ORIENTED_EDGE('',*,*,#10221,.F.);
#14187=ORIENTED_EDGE('',*,*,#10159,.F.);
#14188=ORIENTED_EDGE('',*,*,#10153,.F.);
#14189=ORIENTED_EDGE('',*,*,#10156,.F.);
#14190=ORIENTED_EDGE('',*,*,#10204,.F.);
#14191=ORIENTED_EDGE('',*,*,#10166,.F.);
#14192=ORIENTED_EDGE('',*,*,#10187,.F.);
#14193=ORIENTED_EDGE('',*,*,#10222,.F.);
#14194=ORIENTED_EDGE('',*,*,#10194,.F.);
#14195=ORIENTED_EDGE('',*,*,#10219,.T.);
#14196=ORIENTED_EDGE('',*,*,#10174,.F.);
#14197=ORIENTED_EDGE('',*,*,#10223,.F.);
#14198=ORIENTED_EDGE('',*,*,#10180,.F.);
#14199=ORIENTED_EDGE('',*,*,#10218,.T.);
#14200=ORIENTED_EDGE('',*,*,#10160,.F.);
#14201=ORIENTED_EDGE('',*,*,#10221,.T.);
#14202=ORIENTED_EDGE('',*,*,#10202,.F.);
#14203=ORIENTED_EDGE('',*,*,#10224,.F.);
#14204=ORIENTED_EDGE('',*,*,#10186,.F.);
#14205=ORIENTED_EDGE('',*,*,#10208,.F.);
#14206=ORIENTED_EDGE('',*,*,#10195,.F.);
#14207=ORIENTED_EDGE('',*,*,#10222,.T.);
#14208=ORIENTED_EDGE('',*,*,#10173,.F.);
#14209=ORIENTED_EDGE('',*,*,#10209,.F.);
#14210=ORIENTED_EDGE('',*,*,#10181,.F.);
#14211=ORIENTED_EDGE('',*,*,#10223,.T.);
#14212=ORIENTED_EDGE('',*,*,#10161,.F.);
#14213=ORIENTED_EDGE('',*,*,#10224,.T.);
#14214=ORIENTED_EDGE('',*,*,#10201,.F.);
#14215=ORIENTED_EDGE('',*,*,#10210,.F.);
#14216=ORIENTED_EDGE('',*,*,#10146,.F.);
#14217=ORIENTED_EDGE('',*,*,#10225,.T.);
#14218=ORIENTED_EDGE('',*,*,#10226,.T.);
#14219=ORIENTED_EDGE('',*,*,#10132,.T.);
#14220=ORIENTED_EDGE('',*,*,#10129,.T.);
#14221=ORIENTED_EDGE('',*,*,#10126,.T.);
#14222=ORIENTED_EDGE('',*,*,#10123,.T.);
#14223=ORIENTED_EDGE('',*,*,#10120,.T.);
#14224=ORIENTED_EDGE('',*,*,#10117,.T.);
#14225=ORIENTED_EDGE('',*,*,#10114,.T.);
#14226=ORIENTED_EDGE('',*,*,#10111,.T.);
#14227=ORIENTED_EDGE('',*,*,#10227,.T.);
#14228=ORIENTED_EDGE('',*,*,#10228,.F.);
#14229=ORIENTED_EDGE('',*,*,#10229,.F.);
#14230=ORIENTED_EDGE('',*,*,#10107,.F.);
#14231=ORIENTED_EDGE('',*,*,#10104,.F.);
#14232=ORIENTED_EDGE('',*,*,#10101,.F.);
#14233=ORIENTED_EDGE('',*,*,#10211,.T.);
#14234=ORIENTED_EDGE('',*,*,#10134,.F.);
#14235=ORIENTED_EDGE('',*,*,#10138,.F.);
#14236=ORIENTED_EDGE('',*,*,#10141,.F.);
#14237=ORIENTED_EDGE('',*,*,#10147,.F.);
#14238=ORIENTED_EDGE('',*,*,#10136,.F.);
#14239=ORIENTED_EDGE('',*,*,#10212,.T.);
#14240=ORIENTED_EDGE('',*,*,#10099,.T.);
#14241=ORIENTED_EDGE('',*,*,#10103,.T.);
#14242=ORIENTED_EDGE('',*,*,#10106,.T.);
#14243=ORIENTED_EDGE('',*,*,#10230,.T.);
#14244=ORIENTED_EDGE('',*,*,#10231,.T.);
#14245=ORIENTED_EDGE('',*,*,#10109,.F.);
#14246=ORIENTED_EDGE('',*,*,#10113,.F.);
#14247=ORIENTED_EDGE('',*,*,#10116,.F.);
#14248=ORIENTED_EDGE('',*,*,#10119,.F.);
#14249=ORIENTED_EDGE('',*,*,#10122,.F.);
#14250=ORIENTED_EDGE('',*,*,#10125,.F.);
#14251=ORIENTED_EDGE('',*,*,#10128,.F.);
#14252=ORIENTED_EDGE('',*,*,#10131,.F.);
#14253=ORIENTED_EDGE('',*,*,#10232,.F.);
#14254=ORIENTED_EDGE('',*,*,#10233,.T.);
#14255=ORIENTED_EDGE('',*,*,#10144,.F.);
#14256=ORIENTED_EDGE('',*,*,#10148,.F.);
#14257=ORIENTED_EDGE('',*,*,#10142,.F.);
#14258=ORIENTED_EDGE('',*,*,#10139,.F.);
#14259=ORIENTED_EDGE('',*,*,#10225,.F.);
#14260=ORIENTED_EDGE('',*,*,#10145,.T.);
#14261=ORIENTED_EDGE('',*,*,#10233,.F.);
#14262=ORIENTED_EDGE('',*,*,#10234,.F.);
#14263=ORIENTED_EDGE('',*,*,#10215,.F.);
#14264=ORIENTED_EDGE('',*,*,#10235,.T.);
#14265=ORIENTED_EDGE('',*,*,#10236,.F.);
#14266=ORIENTED_EDGE('',*,*,#10237,.T.);
#14267=ORIENTED_EDGE('',*,*,#10238,.T.);
#14268=ORIENTED_EDGE('',*,*,#10237,.F.);
#14269=ORIENTED_EDGE('',*,*,#10228,.T.);
#14270=ORIENTED_EDGE('',*,*,#10239,.T.);
#14271=ORIENTED_EDGE('',*,*,#10240,.T.);
#14272=ORIENTED_EDGE('',*,*,#10130,.T.);
#14273=ORIENTED_EDGE('',*,*,#10226,.F.);
#14274=ORIENTED_EDGE('',*,*,#10234,.T.);
#14275=ORIENTED_EDGE('',*,*,#10232,.T.);
#14276=ORIENTED_EDGE('',*,*,#10231,.F.);
#14277=ORIENTED_EDGE('',*,*,#10239,.F.);
#14278=ORIENTED_EDGE('',*,*,#10227,.F.);
#14279=ORIENTED_EDGE('',*,*,#10110,.F.);
#14280=ORIENTED_EDGE('',*,*,#10238,.F.);
#14281=ORIENTED_EDGE('',*,*,#10241,.T.);
#14282=ORIENTED_EDGE('',*,*,#10235,.F.);
#14283=ORIENTED_EDGE('',*,*,#10241,.F.);
#14284=ORIENTED_EDGE('',*,*,#10242,.F.);
#14285=ORIENTED_EDGE('',*,*,#10243,.T.);
#14286=ORIENTED_EDGE('',*,*,#10244,.F.);
#14287=ORIENTED_EDGE('',*,*,#10245,.F.);
#14288=ORIENTED_EDGE('',*,*,#10243,.F.);
#14289=ORIENTED_EDGE('',*,*,#10246,.T.);
#14290=ORIENTED_EDGE('',*,*,#10247,.T.);
#14291=ORIENTED_EDGE('',*,*,#10248,.F.);
#14292=ORIENTED_EDGE('',*,*,#10247,.F.);
#14293=ORIENTED_EDGE('',*,*,#10249,.T.);
#14294=ORIENTED_EDGE('',*,*,#10250,.T.);
#14295=ORIENTED_EDGE('',*,*,#10251,.F.);
#14296=ORIENTED_EDGE('',*,*,#10250,.F.);
#14297=ORIENTED_EDGE('',*,*,#10251,.T.);
#14298=ORIENTED_EDGE('',*,*,#10246,.F.);
#14299=ORIENTED_EDGE('',*,*,#10252,.F.);
#14300=ORIENTED_EDGE('',*,*,#10248,.T.);
#14301=ORIENTED_EDGE('',*,*,#10253,.T.);
#14302=ORIENTED_EDGE('',*,*,#10254,.T.);
#14303=ORIENTED_EDGE('',*,*,#10255,.T.);
#14304=ORIENTED_EDGE('',*,*,#10256,.T.);
#14305=ORIENTED_EDGE('',*,*,#10257,.T.);
#14306=ORIENTED_EDGE('',*,*,#10258,.T.);
#14307=ORIENTED_EDGE('',*,*,#10244,.T.);
#14308=ORIENTED_EDGE('',*,*,#10245,.T.);
#14309=ORIENTED_EDGE('',*,*,#10258,.F.);
#14310=ORIENTED_EDGE('',*,*,#10259,.T.);
#14311=ORIENTED_EDGE('',*,*,#10260,.T.);
#14312=ORIENTED_EDGE('',*,*,#10261,.T.);
#14313=ORIENTED_EDGE('',*,*,#10262,.T.);
#14314=ORIENTED_EDGE('',*,*,#10242,.T.);
#14315=ORIENTED_EDGE('',*,*,#10263,.F.);
#14316=ORIENTED_EDGE('',*,*,#10240,.F.);
#14317=ORIENTED_EDGE('',*,*,#10264,.T.);
#14318=ORIENTED_EDGE('',*,*,#10265,.T.);
#14319=ORIENTED_EDGE('',*,*,#10259,.F.);
#14320=ORIENTED_EDGE('',*,*,#10257,.F.);
#14321=ORIENTED_EDGE('',*,*,#10266,.T.);
#14322=ORIENTED_EDGE('',*,*,#10255,.F.);
#14323=ORIENTED_EDGE('',*,*,#10267,.T.);
#14324=ORIENTED_EDGE('',*,*,#10253,.F.);
#14325=ORIENTED_EDGE('',*,*,#10268,.T.);
#14326=ORIENTED_EDGE('',*,*,#10261,.F.);
#14327=ORIENTED_EDGE('',*,*,#10269,.T.);
#14328=ORIENTED_EDGE('',*,*,#10270,.T.);
#14329=ORIENTED_EDGE('',*,*,#10264,.F.);
#14330=ORIENTED_EDGE('',*,*,#10271,.F.);
#14331=ORIENTED_EDGE('',*,*,#10265,.F.);
#14332=ORIENTED_EDGE('',*,*,#10270,.F.);
#14333=ORIENTED_EDGE('',*,*,#10272,.T.);
#14334=ORIENTED_EDGE('',*,*,#10273,.T.);
#14335=ORIENTED_EDGE('',*,*,#10274,.F.);
#14336=ORIENTED_EDGE('',*,*,#10266,.F.);
#14337=ORIENTED_EDGE('',*,*,#10275,.F.);
#14338=ORIENTED_EDGE('',*,*,#10273,.F.);
#14339=ORIENTED_EDGE('',*,*,#10276,.T.);
#14340=ORIENTED_EDGE('',*,*,#10277,.T.);
#14341=ORIENTED_EDGE('',*,*,#10278,.F.);
#14342=ORIENTED_EDGE('',*,*,#10267,.F.);
#14343=ORIENTED_EDGE('',*,*,#10279,.F.);
#14344=ORIENTED_EDGE('',*,*,#10277,.F.);
#14345=ORIENTED_EDGE('',*,*,#10280,.T.);
#14346=ORIENTED_EDGE('',*,*,#10281,.T.);
#14347=ORIENTED_EDGE('',*,*,#10282,.F.);
#14348=ORIENTED_EDGE('',*,*,#10268,.F.);
#14349=ORIENTED_EDGE('',*,*,#10283,.F.);
#14350=ORIENTED_EDGE('',*,*,#10281,.F.);
#14351=ORIENTED_EDGE('',*,*,#10252,.T.);
#14352=ORIENTED_EDGE('',*,*,#10284,.T.);
#14353=ORIENTED_EDGE('',*,*,#10285,.T.);
#14354=ORIENTED_EDGE('',*,*,#10284,.F.);
#14355=ORIENTED_EDGE('',*,*,#10286,.T.);
#14356=ORIENTED_EDGE('',*,*,#10287,.F.);
#14357=ORIENTED_EDGE('',*,*,#10288,.F.);
#14358=ORIENTED_EDGE('',*,*,#10289,.T.);
#14359=ORIENTED_EDGE('',*,*,#10290,.T.);
#14360=ORIENTED_EDGE('',*,*,#10289,.F.);
#14361=ORIENTED_EDGE('',*,*,#10291,.F.);
#14362=ORIENTED_EDGE('',*,*,#10292,.T.);
#14363=ORIENTED_EDGE('',*,*,#10293,.T.);
#14364=ORIENTED_EDGE('',*,*,#10292,.F.);
#14365=ORIENTED_EDGE('',*,*,#10294,.F.);
#14366=ORIENTED_EDGE('',*,*,#10295,.T.);
#14367=ORIENTED_EDGE('',*,*,#10296,.T.);
#14368=ORIENTED_EDGE('',*,*,#10295,.F.);
#14369=ORIENTED_EDGE('',*,*,#10297,.F.);
#14370=ORIENTED_EDGE('',*,*,#10298,.T.);
#14371=ORIENTED_EDGE('',*,*,#10299,.T.);
#14372=ORIENTED_EDGE('',*,*,#10298,.F.);
#14373=ORIENTED_EDGE('',*,*,#10300,.F.);
#14374=ORIENTED_EDGE('',*,*,#10301,.T.);
#14375=ORIENTED_EDGE('',*,*,#10302,.T.);
#14376=ORIENTED_EDGE('',*,*,#10301,.F.);
#14377=ORIENTED_EDGE('',*,*,#10303,.F.);
#14378=ORIENTED_EDGE('',*,*,#10304,.T.);
#14379=ORIENTED_EDGE('',*,*,#10305,.T.);
#14380=ORIENTED_EDGE('',*,*,#10304,.F.);
#14381=ORIENTED_EDGE('',*,*,#10306,.F.);
#14382=ORIENTED_EDGE('',*,*,#10307,.T.);
#14383=ORIENTED_EDGE('',*,*,#10308,.T.);
#14384=ORIENTED_EDGE('',*,*,#10307,.F.);
#14385=ORIENTED_EDGE('',*,*,#10309,.F.);
#14386=ORIENTED_EDGE('',*,*,#10310,.T.);
#14387=ORIENTED_EDGE('',*,*,#10311,.T.);
#14388=ORIENTED_EDGE('',*,*,#10310,.F.);
#14389=ORIENTED_EDGE('',*,*,#10312,.F.);
#14390=ORIENTED_EDGE('',*,*,#10313,.T.);
#14391=ORIENTED_EDGE('',*,*,#10314,.T.);
#14392=ORIENTED_EDGE('',*,*,#10313,.F.);
#14393=ORIENTED_EDGE('',*,*,#10315,.F.);
#14394=ORIENTED_EDGE('',*,*,#10316,.T.);
#14395=ORIENTED_EDGE('',*,*,#10317,.T.);
#14396=ORIENTED_EDGE('',*,*,#10316,.F.);
#14397=ORIENTED_EDGE('',*,*,#10318,.F.);
#14398=ORIENTED_EDGE('',*,*,#10319,.T.);
#14399=ORIENTED_EDGE('',*,*,#10320,.T.);
#14400=ORIENTED_EDGE('',*,*,#10319,.F.);
#14401=ORIENTED_EDGE('',*,*,#10321,.F.);
#14402=ORIENTED_EDGE('',*,*,#10322,.T.);
#14403=ORIENTED_EDGE('',*,*,#10323,.T.);
#14404=ORIENTED_EDGE('',*,*,#10322,.F.);
#14405=ORIENTED_EDGE('',*,*,#10324,.F.);
#14406=ORIENTED_EDGE('',*,*,#10325,.T.);
#14407=ORIENTED_EDGE('',*,*,#10326,.T.);
#14408=ORIENTED_EDGE('',*,*,#10325,.F.);
#14409=ORIENTED_EDGE('',*,*,#10327,.F.);
#14410=ORIENTED_EDGE('',*,*,#10328,.T.);
#14411=ORIENTED_EDGE('',*,*,#10329,.T.);
#14412=ORIENTED_EDGE('',*,*,#10328,.F.);
#14413=ORIENTED_EDGE('',*,*,#10330,.F.);
#14414=ORIENTED_EDGE('',*,*,#10331,.T.);
#14415=ORIENTED_EDGE('',*,*,#10332,.T.);
#14416=ORIENTED_EDGE('',*,*,#10331,.F.);
#14417=ORIENTED_EDGE('',*,*,#10333,.F.);
#14418=ORIENTED_EDGE('',*,*,#10334,.T.);
#14419=ORIENTED_EDGE('',*,*,#10335,.T.);
#14420=ORIENTED_EDGE('',*,*,#10334,.F.);
#14421=ORIENTED_EDGE('',*,*,#10336,.F.);
#14422=ORIENTED_EDGE('',*,*,#10337,.T.);
#14423=ORIENTED_EDGE('',*,*,#10338,.T.);
#14424=ORIENTED_EDGE('',*,*,#10337,.F.);
#14425=ORIENTED_EDGE('',*,*,#10339,.F.);
#14426=ORIENTED_EDGE('',*,*,#10340,.T.);
#14427=ORIENTED_EDGE('',*,*,#10341,.T.);
#14428=ORIENTED_EDGE('',*,*,#10340,.F.);
#14429=ORIENTED_EDGE('',*,*,#10342,.F.);
#14430=ORIENTED_EDGE('',*,*,#10343,.T.);
#14431=ORIENTED_EDGE('',*,*,#10344,.T.);
#14432=ORIENTED_EDGE('',*,*,#10343,.F.);
#14433=ORIENTED_EDGE('',*,*,#10345,.F.);
#14434=ORIENTED_EDGE('',*,*,#10346,.T.);
#14435=ORIENTED_EDGE('',*,*,#10347,.T.);
#14436=ORIENTED_EDGE('',*,*,#10346,.F.);
#14437=ORIENTED_EDGE('',*,*,#10348,.F.);
#14438=ORIENTED_EDGE('',*,*,#10349,.T.);
#14439=ORIENTED_EDGE('',*,*,#10350,.T.);
#14440=ORIENTED_EDGE('',*,*,#10349,.F.);
#14441=ORIENTED_EDGE('',*,*,#10351,.F.);
#14442=ORIENTED_EDGE('',*,*,#10352,.T.);
#14443=ORIENTED_EDGE('',*,*,#10353,.T.);
#14444=ORIENTED_EDGE('',*,*,#10352,.F.);
#14445=ORIENTED_EDGE('',*,*,#10354,.F.);
#14446=ORIENTED_EDGE('',*,*,#10355,.T.);
#14447=ORIENTED_EDGE('',*,*,#10356,.T.);
#14448=ORIENTED_EDGE('',*,*,#10355,.F.);
#14449=ORIENTED_EDGE('',*,*,#10357,.F.);
#14450=ORIENTED_EDGE('',*,*,#10358,.T.);
#14451=ORIENTED_EDGE('',*,*,#10359,.T.);
#14452=ORIENTED_EDGE('',*,*,#10358,.F.);
#14453=ORIENTED_EDGE('',*,*,#10360,.F.);
#14454=ORIENTED_EDGE('',*,*,#10361,.T.);
#14455=ORIENTED_EDGE('',*,*,#10362,.T.);
#14456=ORIENTED_EDGE('',*,*,#10361,.F.);
#14457=ORIENTED_EDGE('',*,*,#10363,.F.);
#14458=ORIENTED_EDGE('',*,*,#10364,.T.);
#14459=ORIENTED_EDGE('',*,*,#10365,.T.);
#14460=ORIENTED_EDGE('',*,*,#10364,.F.);
#14461=ORIENTED_EDGE('',*,*,#10366,.F.);
#14462=ORIENTED_EDGE('',*,*,#10367,.T.);
#14463=ORIENTED_EDGE('',*,*,#10368,.T.);
#14464=ORIENTED_EDGE('',*,*,#10367,.F.);
#14465=ORIENTED_EDGE('',*,*,#10369,.F.);
#14466=ORIENTED_EDGE('',*,*,#10370,.T.);
#14467=ORIENTED_EDGE('',*,*,#10371,.T.);
#14468=ORIENTED_EDGE('',*,*,#10370,.F.);
#14469=ORIENTED_EDGE('',*,*,#10372,.F.);
#14470=ORIENTED_EDGE('',*,*,#10373,.T.);
#14471=ORIENTED_EDGE('',*,*,#10374,.T.);
#14472=ORIENTED_EDGE('',*,*,#10373,.F.);
#14473=ORIENTED_EDGE('',*,*,#10375,.F.);
#14474=ORIENTED_EDGE('',*,*,#10376,.T.);
#14475=ORIENTED_EDGE('',*,*,#10377,.T.);
#14476=ORIENTED_EDGE('',*,*,#10376,.F.);
#14477=ORIENTED_EDGE('',*,*,#10378,.F.);
#14478=ORIENTED_EDGE('',*,*,#10379,.T.);
#14479=ORIENTED_EDGE('',*,*,#10380,.T.);
#14480=ORIENTED_EDGE('',*,*,#10379,.F.);
#14481=ORIENTED_EDGE('',*,*,#10381,.F.);
#14482=ORIENTED_EDGE('',*,*,#10382,.T.);
#14483=ORIENTED_EDGE('',*,*,#10383,.T.);
#14484=ORIENTED_EDGE('',*,*,#10382,.F.);
#14485=ORIENTED_EDGE('',*,*,#10384,.F.);
#14486=ORIENTED_EDGE('',*,*,#10385,.T.);
#14487=ORIENTED_EDGE('',*,*,#10386,.T.);
#14488=ORIENTED_EDGE('',*,*,#10385,.F.);
#14489=ORIENTED_EDGE('',*,*,#10387,.F.);
#14490=ORIENTED_EDGE('',*,*,#10388,.T.);
#14491=ORIENTED_EDGE('',*,*,#10389,.T.);
#14492=ORIENTED_EDGE('',*,*,#10388,.F.);
#14493=ORIENTED_EDGE('',*,*,#10390,.F.);
#14494=ORIENTED_EDGE('',*,*,#10391,.T.);
#14495=ORIENTED_EDGE('',*,*,#10392,.T.);
#14496=ORIENTED_EDGE('',*,*,#10391,.F.);
#14497=ORIENTED_EDGE('',*,*,#10393,.F.);
#14498=ORIENTED_EDGE('',*,*,#10394,.T.);
#14499=ORIENTED_EDGE('',*,*,#10395,.T.);
#14500=ORIENTED_EDGE('',*,*,#10394,.F.);
#14501=ORIENTED_EDGE('',*,*,#10396,.F.);
#14502=ORIENTED_EDGE('',*,*,#10397,.T.);
#14503=ORIENTED_EDGE('',*,*,#10398,.T.);
#14504=ORIENTED_EDGE('',*,*,#10397,.F.);
#14505=ORIENTED_EDGE('',*,*,#10399,.F.);
#14506=ORIENTED_EDGE('',*,*,#10400,.T.);
#14507=ORIENTED_EDGE('',*,*,#10401,.T.);
#14508=ORIENTED_EDGE('',*,*,#10400,.F.);
#14509=ORIENTED_EDGE('',*,*,#10402,.F.);
#14510=ORIENTED_EDGE('',*,*,#10403,.T.);
#14511=ORIENTED_EDGE('',*,*,#10404,.T.);
#14512=ORIENTED_EDGE('',*,*,#10403,.F.);
#14513=ORIENTED_EDGE('',*,*,#10405,.F.);
#14514=ORIENTED_EDGE('',*,*,#10406,.T.);
#14515=ORIENTED_EDGE('',*,*,#10407,.T.);
#14516=ORIENTED_EDGE('',*,*,#10406,.F.);
#14517=ORIENTED_EDGE('',*,*,#10408,.F.);
#14518=ORIENTED_EDGE('',*,*,#10409,.T.);
#14519=ORIENTED_EDGE('',*,*,#10410,.T.);
#14520=ORIENTED_EDGE('',*,*,#10409,.F.);
#14521=ORIENTED_EDGE('',*,*,#10411,.F.);
#14522=ORIENTED_EDGE('',*,*,#10412,.T.);
#14523=ORIENTED_EDGE('',*,*,#10413,.T.);
#14524=ORIENTED_EDGE('',*,*,#10412,.F.);
#14525=ORIENTED_EDGE('',*,*,#10414,.F.);
#14526=ORIENTED_EDGE('',*,*,#10415,.T.);
#14527=ORIENTED_EDGE('',*,*,#10416,.T.);
#14528=ORIENTED_EDGE('',*,*,#10415,.F.);
#14529=ORIENTED_EDGE('',*,*,#10417,.F.);
#14530=ORIENTED_EDGE('',*,*,#10418,.T.);
#14531=ORIENTED_EDGE('',*,*,#10419,.T.);
#14532=ORIENTED_EDGE('',*,*,#10418,.F.);
#14533=ORIENTED_EDGE('',*,*,#10420,.F.);
#14534=ORIENTED_EDGE('',*,*,#10421,.T.);
#14535=ORIENTED_EDGE('',*,*,#10422,.T.);
#14536=ORIENTED_EDGE('',*,*,#10421,.F.);
#14537=ORIENTED_EDGE('',*,*,#10423,.F.);
#14538=ORIENTED_EDGE('',*,*,#10424,.T.);
#14539=ORIENTED_EDGE('',*,*,#10425,.T.);
#14540=ORIENTED_EDGE('',*,*,#10424,.F.);
#14541=ORIENTED_EDGE('',*,*,#10426,.F.);
#14542=ORIENTED_EDGE('',*,*,#10427,.T.);
#14543=ORIENTED_EDGE('',*,*,#10428,.T.);
#14544=ORIENTED_EDGE('',*,*,#10427,.F.);
#14545=ORIENTED_EDGE('',*,*,#10429,.F.);
#14546=ORIENTED_EDGE('',*,*,#10430,.T.);
#14547=ORIENTED_EDGE('',*,*,#10431,.T.);
#14548=ORIENTED_EDGE('',*,*,#10430,.F.);
#14549=ORIENTED_EDGE('',*,*,#10432,.F.);
#14550=ORIENTED_EDGE('',*,*,#10433,.T.);
#14551=ORIENTED_EDGE('',*,*,#10434,.T.);
#14552=ORIENTED_EDGE('',*,*,#10433,.F.);
#14553=ORIENTED_EDGE('',*,*,#10435,.F.);
#14554=ORIENTED_EDGE('',*,*,#10436,.T.);
#14555=ORIENTED_EDGE('',*,*,#10437,.T.);
#14556=ORIENTED_EDGE('',*,*,#10436,.F.);
#14557=ORIENTED_EDGE('',*,*,#10438,.F.);
#14558=ORIENTED_EDGE('',*,*,#10439,.T.);
#14559=ORIENTED_EDGE('',*,*,#10440,.T.);
#14560=ORIENTED_EDGE('',*,*,#10439,.F.);
#14561=ORIENTED_EDGE('',*,*,#10441,.F.);
#14562=ORIENTED_EDGE('',*,*,#10442,.T.);
#14563=ORIENTED_EDGE('',*,*,#10443,.T.);
#14564=ORIENTED_EDGE('',*,*,#10442,.F.);
#14565=ORIENTED_EDGE('',*,*,#10444,.F.);
#14566=ORIENTED_EDGE('',*,*,#10445,.T.);
#14567=ORIENTED_EDGE('',*,*,#10446,.T.);
#14568=ORIENTED_EDGE('',*,*,#10445,.F.);
#14569=ORIENTED_EDGE('',*,*,#10447,.F.);
#14570=ORIENTED_EDGE('',*,*,#10448,.T.);
#14571=ORIENTED_EDGE('',*,*,#10449,.T.);
#14572=ORIENTED_EDGE('',*,*,#10448,.F.);
#14573=ORIENTED_EDGE('',*,*,#10450,.F.);
#14574=ORIENTED_EDGE('',*,*,#10451,.T.);
#14575=ORIENTED_EDGE('',*,*,#10452,.T.);
#14576=ORIENTED_EDGE('',*,*,#10451,.F.);
#14577=ORIENTED_EDGE('',*,*,#10453,.F.);
#14578=ORIENTED_EDGE('',*,*,#10454,.T.);
#14579=ORIENTED_EDGE('',*,*,#10455,.T.);
#14580=ORIENTED_EDGE('',*,*,#10454,.F.);
#14581=ORIENTED_EDGE('',*,*,#10456,.F.);
#14582=ORIENTED_EDGE('',*,*,#10457,.T.);
#14583=ORIENTED_EDGE('',*,*,#10458,.T.);
#14584=ORIENTED_EDGE('',*,*,#10457,.F.);
#14585=ORIENTED_EDGE('',*,*,#10459,.F.);
#14586=ORIENTED_EDGE('',*,*,#10460,.T.);
#14587=ORIENTED_EDGE('',*,*,#10461,.T.);
#14588=ORIENTED_EDGE('',*,*,#10460,.F.);
#14589=ORIENTED_EDGE('',*,*,#10462,.F.);
#14590=ORIENTED_EDGE('',*,*,#10463,.T.);
#14591=ORIENTED_EDGE('',*,*,#10464,.T.);
#14592=ORIENTED_EDGE('',*,*,#10463,.F.);
#14593=ORIENTED_EDGE('',*,*,#10465,.F.);
#14594=ORIENTED_EDGE('',*,*,#10466,.T.);
#14595=ORIENTED_EDGE('',*,*,#10467,.T.);
#14596=ORIENTED_EDGE('',*,*,#10466,.F.);
#14597=ORIENTED_EDGE('',*,*,#10468,.F.);
#14598=ORIENTED_EDGE('',*,*,#10469,.T.);
#14599=ORIENTED_EDGE('',*,*,#10470,.T.);
#14600=ORIENTED_EDGE('',*,*,#10469,.F.);
#14601=ORIENTED_EDGE('',*,*,#10471,.F.);
#14602=ORIENTED_EDGE('',*,*,#10472,.T.);
#14603=ORIENTED_EDGE('',*,*,#10473,.T.);
#14604=ORIENTED_EDGE('',*,*,#10472,.F.);
#14605=ORIENTED_EDGE('',*,*,#10474,.F.);
#14606=ORIENTED_EDGE('',*,*,#10475,.T.);
#14607=ORIENTED_EDGE('',*,*,#10476,.T.);
#14608=ORIENTED_EDGE('',*,*,#10475,.F.);
#14609=ORIENTED_EDGE('',*,*,#10477,.F.);
#14610=ORIENTED_EDGE('',*,*,#10478,.T.);
#14611=ORIENTED_EDGE('',*,*,#10479,.T.);
#14612=ORIENTED_EDGE('',*,*,#10478,.F.);
#14613=ORIENTED_EDGE('',*,*,#10480,.F.);
#14614=ORIENTED_EDGE('',*,*,#10481,.T.);
#14615=ORIENTED_EDGE('',*,*,#10482,.T.);
#14616=ORIENTED_EDGE('',*,*,#10481,.F.);
#14617=ORIENTED_EDGE('',*,*,#10483,.F.);
#14618=ORIENTED_EDGE('',*,*,#10484,.T.);
#14619=ORIENTED_EDGE('',*,*,#10485,.T.);
#14620=ORIENTED_EDGE('',*,*,#10484,.F.);
#14621=ORIENTED_EDGE('',*,*,#10486,.F.);
#14622=ORIENTED_EDGE('',*,*,#10487,.T.);
#14623=ORIENTED_EDGE('',*,*,#10488,.T.);
#14624=ORIENTED_EDGE('',*,*,#10487,.F.);
#14625=ORIENTED_EDGE('',*,*,#10489,.F.);
#14626=ORIENTED_EDGE('',*,*,#10490,.T.);
#14627=ORIENTED_EDGE('',*,*,#10491,.T.);
#14628=ORIENTED_EDGE('',*,*,#10490,.F.);
#14629=ORIENTED_EDGE('',*,*,#10492,.F.);
#14630=ORIENTED_EDGE('',*,*,#10493,.T.);
#14631=ORIENTED_EDGE('',*,*,#10494,.T.);
#14632=ORIENTED_EDGE('',*,*,#10493,.F.);
#14633=ORIENTED_EDGE('',*,*,#10495,.F.);
#14634=ORIENTED_EDGE('',*,*,#10496,.T.);
#14635=ORIENTED_EDGE('',*,*,#10497,.T.);
#14636=ORIENTED_EDGE('',*,*,#10496,.F.);
#14637=ORIENTED_EDGE('',*,*,#10498,.F.);
#14638=ORIENTED_EDGE('',*,*,#10499,.T.);
#14639=ORIENTED_EDGE('',*,*,#10500,.T.);
#14640=ORIENTED_EDGE('',*,*,#10499,.F.);
#14641=ORIENTED_EDGE('',*,*,#10501,.F.);
#14642=ORIENTED_EDGE('',*,*,#10502,.T.);
#14643=ORIENTED_EDGE('',*,*,#10503,.T.);
#14644=ORIENTED_EDGE('',*,*,#10502,.F.);
#14645=ORIENTED_EDGE('',*,*,#10504,.F.);
#14646=ORIENTED_EDGE('',*,*,#10505,.T.);
#14647=ORIENTED_EDGE('',*,*,#10506,.T.);
#14648=ORIENTED_EDGE('',*,*,#10505,.F.);
#14649=ORIENTED_EDGE('',*,*,#10507,.F.);
#14650=ORIENTED_EDGE('',*,*,#10508,.T.);
#14651=ORIENTED_EDGE('',*,*,#10509,.T.);
#14652=ORIENTED_EDGE('',*,*,#10508,.F.);
#14653=ORIENTED_EDGE('',*,*,#10510,.F.);
#14654=ORIENTED_EDGE('',*,*,#10511,.T.);
#14655=ORIENTED_EDGE('',*,*,#10512,.T.);
#14656=ORIENTED_EDGE('',*,*,#10511,.F.);
#14657=ORIENTED_EDGE('',*,*,#10513,.F.);
#14658=ORIENTED_EDGE('',*,*,#10514,.T.);
#14659=ORIENTED_EDGE('',*,*,#10515,.T.);
#14660=ORIENTED_EDGE('',*,*,#10514,.F.);
#14661=ORIENTED_EDGE('',*,*,#10516,.F.);
#14662=ORIENTED_EDGE('',*,*,#10517,.T.);
#14663=ORIENTED_EDGE('',*,*,#10518,.T.);
#14664=ORIENTED_EDGE('',*,*,#10517,.F.);
#14665=ORIENTED_EDGE('',*,*,#10519,.F.);
#14666=ORIENTED_EDGE('',*,*,#10520,.T.);
#14667=ORIENTED_EDGE('',*,*,#10521,.T.);
#14668=ORIENTED_EDGE('',*,*,#10520,.F.);
#14669=ORIENTED_EDGE('',*,*,#10522,.F.);
#14670=ORIENTED_EDGE('',*,*,#10523,.T.);
#14671=ORIENTED_EDGE('',*,*,#10524,.T.);
#14672=ORIENTED_EDGE('',*,*,#10523,.F.);
#14673=ORIENTED_EDGE('',*,*,#10525,.F.);
#14674=ORIENTED_EDGE('',*,*,#10526,.T.);
#14675=ORIENTED_EDGE('',*,*,#10527,.T.);
#14676=ORIENTED_EDGE('',*,*,#10526,.F.);
#14677=ORIENTED_EDGE('',*,*,#10528,.F.);
#14678=ORIENTED_EDGE('',*,*,#10529,.T.);
#14679=ORIENTED_EDGE('',*,*,#10530,.T.);
#14680=ORIENTED_EDGE('',*,*,#10529,.F.);
#14681=ORIENTED_EDGE('',*,*,#10531,.F.);
#14682=ORIENTED_EDGE('',*,*,#10532,.T.);
#14683=ORIENTED_EDGE('',*,*,#10533,.T.);
#14684=ORIENTED_EDGE('',*,*,#10532,.F.);
#14685=ORIENTED_EDGE('',*,*,#10534,.F.);
#14686=ORIENTED_EDGE('',*,*,#10535,.T.);
#14687=ORIENTED_EDGE('',*,*,#10536,.T.);
#14688=ORIENTED_EDGE('',*,*,#10535,.F.);
#14689=ORIENTED_EDGE('',*,*,#10537,.F.);
#14690=ORIENTED_EDGE('',*,*,#10538,.T.);
#14691=ORIENTED_EDGE('',*,*,#10539,.T.);
#14692=ORIENTED_EDGE('',*,*,#10538,.F.);
#14693=ORIENTED_EDGE('',*,*,#10540,.F.);
#14694=ORIENTED_EDGE('',*,*,#10541,.T.);
#14695=ORIENTED_EDGE('',*,*,#10542,.T.);
#14696=ORIENTED_EDGE('',*,*,#10541,.F.);
#14697=ORIENTED_EDGE('',*,*,#10543,.F.);
#14698=ORIENTED_EDGE('',*,*,#10544,.T.);
#14699=ORIENTED_EDGE('',*,*,#10545,.T.);
#14700=ORIENTED_EDGE('',*,*,#10544,.F.);
#14701=ORIENTED_EDGE('',*,*,#10546,.F.);
#14702=ORIENTED_EDGE('',*,*,#10547,.T.);
#14703=ORIENTED_EDGE('',*,*,#10548,.T.);
#14704=ORIENTED_EDGE('',*,*,#10547,.F.);
#14705=ORIENTED_EDGE('',*,*,#10549,.F.);
#14706=ORIENTED_EDGE('',*,*,#10550,.T.);
#14707=ORIENTED_EDGE('',*,*,#10551,.T.);
#14708=ORIENTED_EDGE('',*,*,#10550,.F.);
#14709=ORIENTED_EDGE('',*,*,#10552,.F.);
#14710=ORIENTED_EDGE('',*,*,#10553,.T.);
#14711=ORIENTED_EDGE('',*,*,#10554,.T.);
#14712=ORIENTED_EDGE('',*,*,#10553,.F.);
#14713=ORIENTED_EDGE('',*,*,#10555,.F.);
#14714=ORIENTED_EDGE('',*,*,#10287,.T.);
#14715=ORIENTED_EDGE('',*,*,#10555,.T.);
#14716=ORIENTED_EDGE('',*,*,#10552,.T.);
#14717=ORIENTED_EDGE('',*,*,#10549,.T.);
#14718=ORIENTED_EDGE('',*,*,#10546,.T.);
#14719=ORIENTED_EDGE('',*,*,#10543,.T.);
#14720=ORIENTED_EDGE('',*,*,#10540,.T.);
#14721=ORIENTED_EDGE('',*,*,#10537,.T.);
#14722=ORIENTED_EDGE('',*,*,#10534,.T.);
#14723=ORIENTED_EDGE('',*,*,#10531,.T.);
#14724=ORIENTED_EDGE('',*,*,#10528,.T.);
#14725=ORIENTED_EDGE('',*,*,#10525,.T.);
#14726=ORIENTED_EDGE('',*,*,#10522,.T.);
#14727=ORIENTED_EDGE('',*,*,#10519,.T.);
#14728=ORIENTED_EDGE('',*,*,#10516,.T.);
#14729=ORIENTED_EDGE('',*,*,#10513,.T.);
#14730=ORIENTED_EDGE('',*,*,#10510,.T.);
#14731=ORIENTED_EDGE('',*,*,#10507,.T.);
#14732=ORIENTED_EDGE('',*,*,#10504,.T.);
#14733=ORIENTED_EDGE('',*,*,#10501,.T.);
#14734=ORIENTED_EDGE('',*,*,#10498,.T.);
#14735=ORIENTED_EDGE('',*,*,#10495,.T.);
#14736=ORIENTED_EDGE('',*,*,#10492,.T.);
#14737=ORIENTED_EDGE('',*,*,#10489,.T.);
#14738=ORIENTED_EDGE('',*,*,#10486,.T.);
#14739=ORIENTED_EDGE('',*,*,#10483,.T.);
#14740=ORIENTED_EDGE('',*,*,#10480,.T.);
#14741=ORIENTED_EDGE('',*,*,#10477,.T.);
#14742=ORIENTED_EDGE('',*,*,#10474,.T.);
#14743=ORIENTED_EDGE('',*,*,#10471,.T.);
#14744=ORIENTED_EDGE('',*,*,#10468,.T.);
#14745=ORIENTED_EDGE('',*,*,#10465,.T.);
#14746=ORIENTED_EDGE('',*,*,#10462,.T.);
#14747=ORIENTED_EDGE('',*,*,#10459,.T.);
#14748=ORIENTED_EDGE('',*,*,#10456,.T.);
#14749=ORIENTED_EDGE('',*,*,#10453,.T.);
#14750=ORIENTED_EDGE('',*,*,#10450,.T.);
#14751=ORIENTED_EDGE('',*,*,#10447,.T.);
#14752=ORIENTED_EDGE('',*,*,#10444,.T.);
#14753=ORIENTED_EDGE('',*,*,#10441,.T.);
#14754=ORIENTED_EDGE('',*,*,#10438,.T.);
#14755=ORIENTED_EDGE('',*,*,#10435,.T.);
#14756=ORIENTED_EDGE('',*,*,#10432,.T.);
#14757=ORIENTED_EDGE('',*,*,#10429,.T.);
#14758=ORIENTED_EDGE('',*,*,#10426,.T.);
#14759=ORIENTED_EDGE('',*,*,#10423,.T.);
#14760=ORIENTED_EDGE('',*,*,#10420,.T.);
#14761=ORIENTED_EDGE('',*,*,#10417,.T.);
#14762=ORIENTED_EDGE('',*,*,#10414,.T.);
#14763=ORIENTED_EDGE('',*,*,#10411,.T.);
#14764=ORIENTED_EDGE('',*,*,#10408,.T.);
#14765=ORIENTED_EDGE('',*,*,#10405,.T.);
#14766=ORIENTED_EDGE('',*,*,#10402,.T.);
#14767=ORIENTED_EDGE('',*,*,#10399,.T.);
#14768=ORIENTED_EDGE('',*,*,#10396,.T.);
#14769=ORIENTED_EDGE('',*,*,#10393,.T.);
#14770=ORIENTED_EDGE('',*,*,#10390,.T.);
#14771=ORIENTED_EDGE('',*,*,#10387,.T.);
#14772=ORIENTED_EDGE('',*,*,#10384,.T.);
#14773=ORIENTED_EDGE('',*,*,#10381,.T.);
#14774=ORIENTED_EDGE('',*,*,#10378,.T.);
#14775=ORIENTED_EDGE('',*,*,#10375,.T.);
#14776=ORIENTED_EDGE('',*,*,#10372,.T.);
#14777=ORIENTED_EDGE('',*,*,#10369,.T.);
#14778=ORIENTED_EDGE('',*,*,#10366,.T.);
#14779=ORIENTED_EDGE('',*,*,#10363,.T.);
#14780=ORIENTED_EDGE('',*,*,#10360,.T.);
#14781=ORIENTED_EDGE('',*,*,#10357,.T.);
#14782=ORIENTED_EDGE('',*,*,#10354,.T.);
#14783=ORIENTED_EDGE('',*,*,#10351,.T.);
#14784=ORIENTED_EDGE('',*,*,#10348,.T.);
#14785=ORIENTED_EDGE('',*,*,#10345,.T.);
#14786=ORIENTED_EDGE('',*,*,#10342,.T.);
#14787=ORIENTED_EDGE('',*,*,#10339,.T.);
#14788=ORIENTED_EDGE('',*,*,#10336,.T.);
#14789=ORIENTED_EDGE('',*,*,#10333,.T.);
#14790=ORIENTED_EDGE('',*,*,#10330,.T.);
#14791=ORIENTED_EDGE('',*,*,#10327,.T.);
#14792=ORIENTED_EDGE('',*,*,#10324,.T.);
#14793=ORIENTED_EDGE('',*,*,#10321,.T.);
#14794=ORIENTED_EDGE('',*,*,#10318,.T.);
#14795=ORIENTED_EDGE('',*,*,#10315,.T.);
#14796=ORIENTED_EDGE('',*,*,#10312,.T.);
#14797=ORIENTED_EDGE('',*,*,#10309,.T.);
#14798=ORIENTED_EDGE('',*,*,#10306,.T.);
#14799=ORIENTED_EDGE('',*,*,#10303,.T.);
#14800=ORIENTED_EDGE('',*,*,#10300,.T.);
#14801=ORIENTED_EDGE('',*,*,#10297,.T.);
#14802=ORIENTED_EDGE('',*,*,#10294,.T.);
#14803=ORIENTED_EDGE('',*,*,#10291,.T.);
#14804=ORIENTED_EDGE('',*,*,#10288,.T.);
#14805=ORIENTED_EDGE('',*,*,#10269,.F.);
#14806=ORIENTED_EDGE('',*,*,#10276,.F.);
#14807=ORIENTED_EDGE('',*,*,#10280,.F.);
#14808=ORIENTED_EDGE('',*,*,#10272,.F.);
#14809=ORIENTED_EDGE('',*,*,#10249,.F.);
#14810=ORIENTED_EDGE('',*,*,#10554,.F.);
#14811=ORIENTED_EDGE('',*,*,#10286,.F.);
#14812=ORIENTED_EDGE('',*,*,#10290,.F.);
#14813=ORIENTED_EDGE('',*,*,#10293,.F.);
#14814=ORIENTED_EDGE('',*,*,#10296,.F.);
#14815=ORIENTED_EDGE('',*,*,#10299,.F.);
#14816=ORIENTED_EDGE('',*,*,#10302,.F.);
#14817=ORIENTED_EDGE('',*,*,#10305,.F.);
#14818=ORIENTED_EDGE('',*,*,#10308,.F.);
#14819=ORIENTED_EDGE('',*,*,#10311,.F.);
#14820=ORIENTED_EDGE('',*,*,#10314,.F.);
#14821=ORIENTED_EDGE('',*,*,#10317,.F.);
#14822=ORIENTED_EDGE('',*,*,#10320,.F.);
#14823=ORIENTED_EDGE('',*,*,#10323,.F.);
#14824=ORIENTED_EDGE('',*,*,#10326,.F.);
#14825=ORIENTED_EDGE('',*,*,#10329,.F.);
#14826=ORIENTED_EDGE('',*,*,#10332,.F.);
#14827=ORIENTED_EDGE('',*,*,#10335,.F.);
#14828=ORIENTED_EDGE('',*,*,#10338,.F.);
#14829=ORIENTED_EDGE('',*,*,#10341,.F.);
#14830=ORIENTED_EDGE('',*,*,#10344,.F.);
#14831=ORIENTED_EDGE('',*,*,#10347,.F.);
#14832=ORIENTED_EDGE('',*,*,#10350,.F.);
#14833=ORIENTED_EDGE('',*,*,#10353,.F.);
#14834=ORIENTED_EDGE('',*,*,#10356,.F.);
#14835=ORIENTED_EDGE('',*,*,#10359,.F.);
#14836=ORIENTED_EDGE('',*,*,#10362,.F.);
#14837=ORIENTED_EDGE('',*,*,#10365,.F.);
#14838=ORIENTED_EDGE('',*,*,#10368,.F.);
#14839=ORIENTED_EDGE('',*,*,#10371,.F.);
#14840=ORIENTED_EDGE('',*,*,#10374,.F.);
#14841=ORIENTED_EDGE('',*,*,#10377,.F.);
#14842=ORIENTED_EDGE('',*,*,#10380,.F.);
#14843=ORIENTED_EDGE('',*,*,#10383,.F.);
#14844=ORIENTED_EDGE('',*,*,#10386,.F.);
#14845=ORIENTED_EDGE('',*,*,#10389,.F.);
#14846=ORIENTED_EDGE('',*,*,#10392,.F.);
#14847=ORIENTED_EDGE('',*,*,#10395,.F.);
#14848=ORIENTED_EDGE('',*,*,#10398,.F.);
#14849=ORIENTED_EDGE('',*,*,#10401,.F.);
#14850=ORIENTED_EDGE('',*,*,#10404,.F.);
#14851=ORIENTED_EDGE('',*,*,#10407,.F.);
#14852=ORIENTED_EDGE('',*,*,#10410,.F.);
#14853=ORIENTED_EDGE('',*,*,#10413,.F.);
#14854=ORIENTED_EDGE('',*,*,#10416,.F.);
#14855=ORIENTED_EDGE('',*,*,#10419,.F.);
#14856=ORIENTED_EDGE('',*,*,#10422,.F.);
#14857=ORIENTED_EDGE('',*,*,#10425,.F.);
#14858=ORIENTED_EDGE('',*,*,#10428,.F.);
#14859=ORIENTED_EDGE('',*,*,#10431,.F.);
#14860=ORIENTED_EDGE('',*,*,#10434,.F.);
#14861=ORIENTED_EDGE('',*,*,#10437,.F.);
#14862=ORIENTED_EDGE('',*,*,#10440,.F.);
#14863=ORIENTED_EDGE('',*,*,#10443,.F.);
#14864=ORIENTED_EDGE('',*,*,#10446,.F.);
#14865=ORIENTED_EDGE('',*,*,#10449,.F.);
#14866=ORIENTED_EDGE('',*,*,#10452,.F.);
#14867=ORIENTED_EDGE('',*,*,#10455,.F.);
#14868=ORIENTED_EDGE('',*,*,#10458,.F.);
#14869=ORIENTED_EDGE('',*,*,#10461,.F.);
#14870=ORIENTED_EDGE('',*,*,#10464,.F.);
#14871=ORIENTED_EDGE('',*,*,#10467,.F.);
#14872=ORIENTED_EDGE('',*,*,#10470,.F.);
#14873=ORIENTED_EDGE('',*,*,#10473,.F.);
#14874=ORIENTED_EDGE('',*,*,#10476,.F.);
#14875=ORIENTED_EDGE('',*,*,#10479,.F.);
#14876=ORIENTED_EDGE('',*,*,#10482,.F.);
#14877=ORIENTED_EDGE('',*,*,#10485,.F.);
#14878=ORIENTED_EDGE('',*,*,#10488,.F.);
#14879=ORIENTED_EDGE('',*,*,#10491,.F.);
#14880=ORIENTED_EDGE('',*,*,#10494,.F.);
#14881=ORIENTED_EDGE('',*,*,#10497,.F.);
#14882=ORIENTED_EDGE('',*,*,#10500,.F.);
#14883=ORIENTED_EDGE('',*,*,#10503,.F.);
#14884=ORIENTED_EDGE('',*,*,#10506,.F.);
#14885=ORIENTED_EDGE('',*,*,#10509,.F.);
#14886=ORIENTED_EDGE('',*,*,#10512,.F.);
#14887=ORIENTED_EDGE('',*,*,#10515,.F.);
#14888=ORIENTED_EDGE('',*,*,#10518,.F.);
#14889=ORIENTED_EDGE('',*,*,#10521,.F.);
#14890=ORIENTED_EDGE('',*,*,#10524,.F.);
#14891=ORIENTED_EDGE('',*,*,#10527,.F.);
#14892=ORIENTED_EDGE('',*,*,#10530,.F.);
#14893=ORIENTED_EDGE('',*,*,#10533,.F.);
#14894=ORIENTED_EDGE('',*,*,#10536,.F.);
#14895=ORIENTED_EDGE('',*,*,#10539,.F.);
#14896=ORIENTED_EDGE('',*,*,#10542,.F.);
#14897=ORIENTED_EDGE('',*,*,#10545,.F.);
#14898=ORIENTED_EDGE('',*,*,#10548,.F.);
#14899=ORIENTED_EDGE('',*,*,#10551,.F.);
#14900=ORIENTED_EDGE('',*,*,#10254,.F.);
#14901=ORIENTED_EDGE('',*,*,#10278,.T.);
#14902=ORIENTED_EDGE('',*,*,#10279,.T.);
#14903=ORIENTED_EDGE('',*,*,#10262,.F.);
#14904=ORIENTED_EDGE('',*,*,#10282,.T.);
#14905=ORIENTED_EDGE('',*,*,#10283,.T.);
#14906=ORIENTED_EDGE('',*,*,#10260,.F.);
#14907=ORIENTED_EDGE('',*,*,#10271,.T.);
#14908=ORIENTED_EDGE('',*,*,#10256,.F.);
#14909=ORIENTED_EDGE('',*,*,#10274,.T.);
#14910=ORIENTED_EDGE('',*,*,#10275,.T.);
#14911=ORIENTED_EDGE('',*,*,#10105,.T.);
#14912=ORIENTED_EDGE('',*,*,#10229,.T.);
#14913=ORIENTED_EDGE('',*,*,#10263,.T.);
#14914=ORIENTED_EDGE('',*,*,#10230,.F.);
#14915=ORIENTED_EDGE('',*,*,#10236,.T.);
#14916=ORIENTED_EDGE('',*,*,#10556,.T.);
#14917=ORIENTED_EDGE('',*,*,#10285,.F.);
#14918=ORIENTED_EDGE('',*,*,#10557,.F.);
#14919=ORIENTED_EDGE('',*,*,#10558,.T.);
#14920=ORIENTED_EDGE('',*,*,#10559,.T.);
#14921=ORIENTED_EDGE('',*,*,#10560,.T.);
#14922=ORIENTED_EDGE('',*,*,#10556,.F.);
#14923=ORIENTED_EDGE('',*,*,#10560,.F.);
#14924=ORIENTED_EDGE('',*,*,#10561,.F.);
#14925=ORIENTED_EDGE('',*,*,#9977,.T.);
#14926=ORIENTED_EDGE('',*,*,#9980,.T.);
#14927=ORIENTED_EDGE('',*,*,#9983,.T.);
#14928=ORIENTED_EDGE('',*,*,#9986,.T.);
#14929=ORIENTED_EDGE('',*,*,#9989,.T.);
#14930=ORIENTED_EDGE('',*,*,#9992,.T.);
#14931=ORIENTED_EDGE('',*,*,#9995,.T.);
#14932=ORIENTED_EDGE('',*,*,#9998,.T.);
#14933=ORIENTED_EDGE('',*,*,#10001,.T.);
#14934=ORIENTED_EDGE('',*,*,#10004,.T.);
#14935=ORIENTED_EDGE('',*,*,#10007,.T.);
#14936=ORIENTED_EDGE('',*,*,#10010,.T.);
#14937=ORIENTED_EDGE('',*,*,#10013,.T.);
#14938=ORIENTED_EDGE('',*,*,#10016,.T.);
#14939=ORIENTED_EDGE('',*,*,#10019,.T.);
#14940=ORIENTED_EDGE('',*,*,#10022,.T.);
#14941=ORIENTED_EDGE('',*,*,#10025,.T.);
#14942=ORIENTED_EDGE('',*,*,#10562,.T.);
#14943=ORIENTED_EDGE('',*,*,#10030,.T.);
#14944=ORIENTED_EDGE('',*,*,#10563,.T.);
#14945=ORIENTED_EDGE('',*,*,#10035,.T.);
#14946=ORIENTED_EDGE('',*,*,#10564,.F.);
#14947=ORIENTED_EDGE('',*,*,#10037,.F.);
#14948=ORIENTED_EDGE('',*,*,#10041,.F.);
#14949=ORIENTED_EDGE('',*,*,#10044,.F.);
#14950=ORIENTED_EDGE('',*,*,#10047,.F.);
#14951=ORIENTED_EDGE('',*,*,#10050,.F.);
#14952=ORIENTED_EDGE('',*,*,#10053,.F.);
#14953=ORIENTED_EDGE('',*,*,#10056,.F.);
#14954=ORIENTED_EDGE('',*,*,#10059,.F.);
#14955=ORIENTED_EDGE('',*,*,#10062,.F.);
#14956=ORIENTED_EDGE('',*,*,#10065,.F.);
#14957=ORIENTED_EDGE('',*,*,#10068,.F.);
#14958=ORIENTED_EDGE('',*,*,#10071,.F.);
#14959=ORIENTED_EDGE('',*,*,#10074,.F.);
#14960=ORIENTED_EDGE('',*,*,#10077,.F.);
#14961=ORIENTED_EDGE('',*,*,#10080,.F.);
#14962=ORIENTED_EDGE('',*,*,#10083,.F.);
#14963=ORIENTED_EDGE('',*,*,#10086,.F.);
#14964=ORIENTED_EDGE('',*,*,#10089,.F.);
#14965=ORIENTED_EDGE('',*,*,#10092,.F.);
#14966=ORIENTED_EDGE('',*,*,#10565,.F.);
#14967=ORIENTED_EDGE('',*,*,#10097,.F.);
#14968=ORIENTED_EDGE('',*,*,#10094,.T.);
#14969=ORIENTED_EDGE('',*,*,#10565,.T.);
#14970=ORIENTED_EDGE('',*,*,#10091,.F.);
#14971=ORIENTED_EDGE('',*,*,#10566,.F.);
#14972=ORIENTED_EDGE('',*,*,#10567,.F.);
#14973=ORIENTED_EDGE('',*,*,#10095,.T.);
#14974=ORIENTED_EDGE('',*,*,#10566,.T.);
#14975=ORIENTED_EDGE('',*,*,#10093,.T.);
#14976=ORIENTED_EDGE('',*,*,#10090,.T.);
#14977=ORIENTED_EDGE('',*,*,#10087,.T.);
#14978=ORIENTED_EDGE('',*,*,#10084,.T.);
#14979=ORIENTED_EDGE('',*,*,#10081,.T.);
#14980=ORIENTED_EDGE('',*,*,#10078,.T.);
#14981=ORIENTED_EDGE('',*,*,#10075,.T.);
#14982=ORIENTED_EDGE('',*,*,#10072,.T.);
#14983=ORIENTED_EDGE('',*,*,#10069,.T.);
#14984=ORIENTED_EDGE('',*,*,#10066,.T.);
#14985=ORIENTED_EDGE('',*,*,#10063,.T.);
#14986=ORIENTED_EDGE('',*,*,#10060,.T.);
#14987=ORIENTED_EDGE('',*,*,#10057,.T.);
#14988=ORIENTED_EDGE('',*,*,#10054,.T.);
#14989=ORIENTED_EDGE('',*,*,#10051,.T.);
#14990=ORIENTED_EDGE('',*,*,#10048,.T.);
#14991=ORIENTED_EDGE('',*,*,#10045,.T.);
#14992=ORIENTED_EDGE('',*,*,#10042,.T.);
#14993=ORIENTED_EDGE('',*,*,#10039,.T.);
#14994=ORIENTED_EDGE('',*,*,#10568,.F.);
#14995=ORIENTED_EDGE('',*,*,#10033,.F.);
#14996=ORIENTED_EDGE('',*,*,#10028,.F.);
#14997=ORIENTED_EDGE('',*,*,#10569,.F.);
#14998=ORIENTED_EDGE('',*,*,#10026,.F.);
#14999=ORIENTED_EDGE('',*,*,#10023,.F.);
#15000=ORIENTED_EDGE('',*,*,#10020,.F.);
#15001=ORIENTED_EDGE('',*,*,#10017,.F.);
#15002=ORIENTED_EDGE('',*,*,#10014,.F.);
#15003=ORIENTED_EDGE('',*,*,#10011,.F.);
#15004=ORIENTED_EDGE('',*,*,#10008,.F.);
#15005=ORIENTED_EDGE('',*,*,#10005,.F.);
#15006=ORIENTED_EDGE('',*,*,#10002,.F.);
#15007=ORIENTED_EDGE('',*,*,#9999,.F.);
#15008=ORIENTED_EDGE('',*,*,#9996,.F.);
#15009=ORIENTED_EDGE('',*,*,#9993,.F.);
#15010=ORIENTED_EDGE('',*,*,#9990,.F.);
#15011=ORIENTED_EDGE('',*,*,#9987,.F.);
#15012=ORIENTED_EDGE('',*,*,#9984,.F.);
#15013=ORIENTED_EDGE('',*,*,#9981,.F.);
#15014=ORIENTED_EDGE('',*,*,#9978,.F.);
#15015=ORIENTED_EDGE('',*,*,#9975,.F.);
#15016=ORIENTED_EDGE('',*,*,#10570,.F.);
#15017=ORIENTED_EDGE('',*,*,#10568,.T.);
#15018=ORIENTED_EDGE('',*,*,#10038,.T.);
#15019=ORIENTED_EDGE('',*,*,#10564,.T.);
#15020=ORIENTED_EDGE('',*,*,#10034,.T.);
#15021=ORIENTED_EDGE('',*,*,#10567,.T.);
#15022=ORIENTED_EDGE('',*,*,#10571,.T.);
#15023=ORIENTED_EDGE('',*,*,#9973,.T.);
#15024=ORIENTED_EDGE('',*,*,#10561,.T.);
#15025=ORIENTED_EDGE('',*,*,#10096,.T.);
#15026=ORIENTED_EDGE('',*,*,#10031,.T.);
#15027=ORIENTED_EDGE('',*,*,#10563,.F.);
#15028=ORIENTED_EDGE('',*,*,#10572,.T.);
#15029=ORIENTED_EDGE('',*,*,#10570,.T.);
#15030=ORIENTED_EDGE('',*,*,#10573,.T.);
#15031=ORIENTED_EDGE('',*,*,#10571,.F.);
#15032=ORIENTED_EDGE('',*,*,#10572,.F.);
#15033=ORIENTED_EDGE('',*,*,#10029,.F.);
#15034=ORIENTED_EDGE('',*,*,#10032,.F.);
#15035=ORIENTED_EDGE('',*,*,#10574,.T.);
#15036=ORIENTED_EDGE('',*,*,#10575,.F.);
#15037=ORIENTED_EDGE('',*,*,#10574,.F.);
#15038=ORIENTED_EDGE('',*,*,#10573,.F.);
#15039=ORIENTED_EDGE('',*,*,#9974,.F.);
#15040=ORIENTED_EDGE('',*,*,#10576,.T.);
#15041=ORIENTED_EDGE('',*,*,#10577,.F.);
#15042=ORIENTED_EDGE('',*,*,#10576,.F.);
#15043=ORIENTED_EDGE('',*,*,#10558,.F.);
#15044=ORIENTED_EDGE('',*,*,#10559,.F.);
#15045=ORIENTED_EDGE('',*,*,#10578,.T.);
#15046=ORIENTED_EDGE('',*,*,#10579,.F.);
#15047=ORIENTED_EDGE('',*,*,#10578,.F.);
#15048=ORIENTED_EDGE('',*,*,#10580,.F.);
#15049=ORIENTED_EDGE('',*,*,#10581,.T.);
#15050=ORIENTED_EDGE('',*,*,#10582,.F.);
#15051=ORIENTED_EDGE('',*,*,#10581,.F.);
#15052=ORIENTED_EDGE('',*,*,#10557,.T.);
#15053=ORIENTED_EDGE('',*,*,#10583,.T.);
#15054=ORIENTED_EDGE('',*,*,#10580,.T.);
#15055=ORIENTED_EDGE('',*,*,#10583,.F.);
#15056=ORIENTED_EDGE('',*,*,#10579,.T.);
#15057=ORIENTED_EDGE('',*,*,#10577,.T.);
#15058=ORIENTED_EDGE('',*,*,#10582,.T.);
#15059=ORIENTED_EDGE('',*,*,#10575,.T.);
#15060=ORIENTED_EDGE('',*,*,#10027,.T.);
#15061=ORIENTED_EDGE('',*,*,#10562,.F.);
#15062=ORIENTED_EDGE('',*,*,#10024,.F.);
#15063=ORIENTED_EDGE('',*,*,#10569,.T.);
#15064=ORIENTED_EDGE('',*,*,#10584,.F.);
#15065=ORIENTED_EDGE('',*,*,#10585,.T.);
#15066=ORIENTED_EDGE('',*,*,#10586,.T.);
#15067=ORIENTED_EDGE('',*,*,#10585,.F.);
#15068=ORIENTED_EDGE('',*,*,#10587,.T.);
#15069=ORIENTED_EDGE('',*,*,#10588,.T.);
#15070=ORIENTED_EDGE('',*,*,#10589,.T.);
#15071=ORIENTED_EDGE('',*,*,#10590,.F.);
#15072=ORIENTED_EDGE('',*,*,#10589,.F.);
#15073=ORIENTED_EDGE('',*,*,#10591,.T.);
#15074=ORIENTED_EDGE('',*,*,#10592,.T.);
#15075=ORIENTED_EDGE('',*,*,#10591,.F.);
#15076=ORIENTED_EDGE('',*,*,#10588,.F.);
#15077=ORIENTED_EDGE('',*,*,#10593,.F.);
#15078=ORIENTED_EDGE('',*,*,#10594,.F.);
#15079=ORIENTED_EDGE('',*,*,#10595,.F.);
#15080=ORIENTED_EDGE('',*,*,#10596,.F.);
#15081=ORIENTED_EDGE('',*,*,#10597,.F.);
#15082=ORIENTED_EDGE('',*,*,#10598,.F.);
#15083=ORIENTED_EDGE('',*,*,#10599,.F.);
#15084=ORIENTED_EDGE('',*,*,#10600,.F.);
#15085=ORIENTED_EDGE('',*,*,#10594,.T.);
#15086=ORIENTED_EDGE('',*,*,#10601,.T.);
#15087=ORIENTED_EDGE('',*,*,#10602,.F.);
#15088=ORIENTED_EDGE('',*,*,#10603,.F.);
#15089=ORIENTED_EDGE('',*,*,#10595,.T.);
#15090=ORIENTED_EDGE('',*,*,#10600,.T.);
#15091=ORIENTED_EDGE('',*,*,#10604,.F.);
#15092=ORIENTED_EDGE('',*,*,#10605,.F.);
#15093=ORIENTED_EDGE('',*,*,#10596,.T.);
#15094=ORIENTED_EDGE('',*,*,#10603,.T.);
#15095=ORIENTED_EDGE('',*,*,#10606,.F.);
#15096=ORIENTED_EDGE('',*,*,#10607,.F.);
#15097=ORIENTED_EDGE('',*,*,#10597,.T.);
#15098=ORIENTED_EDGE('',*,*,#10605,.T.);
#15099=ORIENTED_EDGE('',*,*,#10608,.F.);
#15100=ORIENTED_EDGE('',*,*,#10609,.F.);
#15101=ORIENTED_EDGE('',*,*,#10598,.T.);
#15102=ORIENTED_EDGE('',*,*,#10607,.T.);
#15103=ORIENTED_EDGE('',*,*,#10610,.F.);
#15104=ORIENTED_EDGE('',*,*,#10601,.F.);
#15105=ORIENTED_EDGE('',*,*,#10593,.T.);
#15106=ORIENTED_EDGE('',*,*,#10609,.T.);
#15107=ORIENTED_EDGE('',*,*,#10611,.F.);
#15108=ORIENTED_EDGE('',*,*,#10612,.F.);
#15109=ORIENTED_EDGE('',*,*,#10613,.F.);
#15110=ORIENTED_EDGE('',*,*,#10614,.F.);
#15111=ORIENTED_EDGE('',*,*,#10615,.F.);
#15112=ORIENTED_EDGE('',*,*,#10616,.F.);
#15113=ORIENTED_EDGE('',*,*,#10617,.F.);
#15114=ORIENTED_EDGE('',*,*,#10618,.F.);
#15115=ORIENTED_EDGE('',*,*,#10619,.F.);
#15116=ORIENTED_EDGE('',*,*,#10620,.F.);
#15117=ORIENTED_EDGE('',*,*,#10621,.F.);
#15118=ORIENTED_EDGE('',*,*,#10622,.F.);
#15119=ORIENTED_EDGE('',*,*,#10623,.F.);
#15120=ORIENTED_EDGE('',*,*,#10624,.F.);
#15121=ORIENTED_EDGE('',*,*,#10612,.T.);
#15122=ORIENTED_EDGE('',*,*,#10625,.T.);
#15123=ORIENTED_EDGE('',*,*,#10626,.F.);
#15124=ORIENTED_EDGE('',*,*,#10627,.F.);
#15125=ORIENTED_EDGE('',*,*,#10613,.T.);
#15126=ORIENTED_EDGE('',*,*,#10624,.T.);
#15127=ORIENTED_EDGE('',*,*,#10628,.F.);
#15128=ORIENTED_EDGE('',*,*,#10629,.F.);
#15129=ORIENTED_EDGE('',*,*,#10614,.T.);
#15130=ORIENTED_EDGE('',*,*,#10627,.T.);
#15131=ORIENTED_EDGE('',*,*,#10630,.F.);
#15132=ORIENTED_EDGE('',*,*,#10631,.F.);
#15133=ORIENTED_EDGE('',*,*,#10615,.T.);
#15134=ORIENTED_EDGE('',*,*,#10629,.T.);
#15135=ORIENTED_EDGE('',*,*,#10632,.F.);
#15136=ORIENTED_EDGE('',*,*,#10633,.F.);
#15137=ORIENTED_EDGE('',*,*,#10616,.T.);
#15138=ORIENTED_EDGE('',*,*,#10631,.T.);
#15139=ORIENTED_EDGE('',*,*,#10634,.F.);
#15140=ORIENTED_EDGE('',*,*,#10635,.F.);
#15141=ORIENTED_EDGE('',*,*,#10617,.T.);
#15142=ORIENTED_EDGE('',*,*,#10633,.T.);
#15143=ORIENTED_EDGE('',*,*,#10636,.F.);
#15144=ORIENTED_EDGE('',*,*,#10637,.F.);
#15145=ORIENTED_EDGE('',*,*,#10618,.T.);
#15146=ORIENTED_EDGE('',*,*,#10635,.T.);
#15147=ORIENTED_EDGE('',*,*,#10638,.F.);
#15148=ORIENTED_EDGE('',*,*,#10639,.F.);
#15149=ORIENTED_EDGE('',*,*,#10619,.T.);
#15150=ORIENTED_EDGE('',*,*,#10637,.T.);
#15151=ORIENTED_EDGE('',*,*,#10640,.F.);
#15152=ORIENTED_EDGE('',*,*,#10641,.F.);
#15153=ORIENTED_EDGE('',*,*,#10620,.T.);
#15154=ORIENTED_EDGE('',*,*,#10639,.T.);
#15155=ORIENTED_EDGE('',*,*,#10642,.F.);
#15156=ORIENTED_EDGE('',*,*,#10643,.F.);
#15157=ORIENTED_EDGE('',*,*,#10621,.T.);
#15158=ORIENTED_EDGE('',*,*,#10641,.T.);
#15159=ORIENTED_EDGE('',*,*,#10644,.F.);
#15160=ORIENTED_EDGE('',*,*,#10645,.F.);
#15161=ORIENTED_EDGE('',*,*,#10622,.T.);
#15162=ORIENTED_EDGE('',*,*,#10643,.T.);
#15163=ORIENTED_EDGE('',*,*,#10646,.F.);
#15164=ORIENTED_EDGE('',*,*,#10625,.F.);
#15165=ORIENTED_EDGE('',*,*,#10611,.T.);
#15166=ORIENTED_EDGE('',*,*,#10645,.T.);
#15167=ORIENTED_EDGE('',*,*,#10647,.F.);
#15168=ORIENTED_EDGE('',*,*,#10648,.F.);
#15169=ORIENTED_EDGE('',*,*,#10649,.T.);
#15170=ORIENTED_EDGE('',*,*,#10650,.T.);
#15171=ORIENTED_EDGE('',*,*,#10651,.F.);
#15172=ORIENTED_EDGE('',*,*,#10652,.F.);
#15173=ORIENTED_EDGE('',*,*,#10653,.F.);
#15174=ORIENTED_EDGE('',*,*,#10647,.T.);
#15175=ORIENTED_EDGE('',*,*,#10654,.F.);
#15176=ORIENTED_EDGE('',*,*,#10655,.F.);
#15177=ORIENTED_EDGE('',*,*,#10656,.F.);
#15178=ORIENTED_EDGE('',*,*,#10652,.T.);
#15179=ORIENTED_EDGE('',*,*,#10657,.F.);
#15180=ORIENTED_EDGE('',*,*,#10658,.F.);
#15181=ORIENTED_EDGE('',*,*,#10659,.F.);
#15182=ORIENTED_EDGE('',*,*,#10660,.T.);
#15183=ORIENTED_EDGE('',*,*,#10661,.F.);
#15184=ORIENTED_EDGE('',*,*,#10662,.F.);
#15185=ORIENTED_EDGE('',*,*,#10663,.F.);
#15186=ORIENTED_EDGE('',*,*,#10658,.T.);
#15187=ORIENTED_EDGE('',*,*,#10664,.F.);
#15188=ORIENTED_EDGE('',*,*,#10665,.T.);
#15189=ORIENTED_EDGE('',*,*,#10666,.F.);
#15190=ORIENTED_EDGE('',*,*,#10667,.F.);
#15191=ORIENTED_EDGE('',*,*,#10662,.T.);
#15192=ORIENTED_EDGE('',*,*,#10668,.F.);
#15193=ORIENTED_EDGE('',*,*,#10669,.F.);
#15194=ORIENTED_EDGE('',*,*,#10670,.F.);
#15195=ORIENTED_EDGE('',*,*,#10671,.F.);
#15196=ORIENTED_EDGE('',*,*,#10672,.F.);
#15197=ORIENTED_EDGE('',*,*,#10673,.T.);
#15198=ORIENTED_EDGE('',*,*,#10674,.F.);
#15199=ORIENTED_EDGE('',*,*,#10675,.F.);
#15200=ORIENTED_EDGE('',*,*,#10676,.F.);
#15201=ORIENTED_EDGE('',*,*,#10669,.T.);
#15202=ORIENTED_EDGE('',*,*,#10677,.F.);
#15203=ORIENTED_EDGE('',*,*,#10678,.T.);
#15204=ORIENTED_EDGE('',*,*,#10679,.T.);
#15205=ORIENTED_EDGE('',*,*,#10680,.T.);
#15206=ORIENTED_EDGE('',*,*,#10681,.T.);
#15207=ORIENTED_EDGE('',*,*,#10678,.F.);
#15208=ORIENTED_EDGE('',*,*,#10681,.F.);
#15209=ORIENTED_EDGE('',*,*,#10682,.T.);
#15210=ORIENTED_EDGE('',*,*,#10683,.T.);
#15211=ORIENTED_EDGE('',*,*,#10679,.F.);
#15212=ORIENTED_EDGE('',*,*,#10683,.F.);
#15213=ORIENTED_EDGE('',*,*,#10684,.T.);
#15214=ORIENTED_EDGE('',*,*,#10685,.T.);
#15215=ORIENTED_EDGE('',*,*,#10686,.T.);
#15216=ORIENTED_EDGE('',*,*,#10687,.F.);
#15217=ORIENTED_EDGE('',*,*,#10688,.F.);
#15218=ORIENTED_EDGE('',*,*,#10689,.T.);
#15219=ORIENTED_EDGE('',*,*,#10690,.T.);
#15220=ORIENTED_EDGE('',*,*,#10689,.F.);
#15221=ORIENTED_EDGE('',*,*,#10691,.F.);
#15222=ORIENTED_EDGE('',*,*,#10692,.T.);
#15223=ORIENTED_EDGE('',*,*,#10693,.T.);
#15224=ORIENTED_EDGE('',*,*,#10694,.T.);
#15225=ORIENTED_EDGE('',*,*,#10695,.T.);
#15226=ORIENTED_EDGE('',*,*,#10692,.F.);
#15227=ORIENTED_EDGE('',*,*,#10696,.F.);
#15228=ORIENTED_EDGE('',*,*,#10697,.T.);
#15229=ORIENTED_EDGE('',*,*,#10698,.T.);
#15230=ORIENTED_EDGE('',*,*,#10697,.F.);
#15231=ORIENTED_EDGE('',*,*,#10699,.F.);
#15232=ORIENTED_EDGE('',*,*,#10687,.T.);
#15233=ORIENTED_EDGE('',*,*,#10699,.T.);
#15234=ORIENTED_EDGE('',*,*,#10696,.T.);
#15235=ORIENTED_EDGE('',*,*,#10691,.T.);
#15236=ORIENTED_EDGE('',*,*,#10688,.T.);
#15237=ORIENTED_EDGE('',*,*,#10680,.F.);
#15238=ORIENTED_EDGE('',*,*,#10682,.F.);
#15239=ORIENTED_EDGE('',*,*,#10700,.F.);
#15240=ORIENTED_EDGE('',*,*,#10685,.F.);
#15241=ORIENTED_EDGE('',*,*,#10701,.F.);
#15242=ORIENTED_EDGE('',*,*,#10694,.F.);
#15243=ORIENTED_EDGE('',*,*,#10702,.F.);
#15244=ORIENTED_EDGE('',*,*,#10703,.F.);
#15245=ORIENTED_EDGE('',*,*,#10704,.F.);
#15246=ORIENTED_EDGE('',*,*,#10705,.F.);
#15247=ORIENTED_EDGE('',*,*,#10706,.T.);
#15248=ORIENTED_EDGE('',*,*,#10707,.T.);
#15249=ORIENTED_EDGE('',*,*,#10708,.T.);
#15250=ORIENTED_EDGE('',*,*,#10709,.T.);
#15251=ORIENTED_EDGE('',*,*,#10710,.T.);
#15252=ORIENTED_EDGE('',*,*,#10711,.T.);
#15253=ORIENTED_EDGE('',*,*,#10712,.F.);
#15254=ORIENTED_EDGE('',*,*,#10713,.F.);
#15255=ORIENTED_EDGE('',*,*,#10695,.F.);
#15256=ORIENTED_EDGE('',*,*,#10714,.F.);
#15257=ORIENTED_EDGE('',*,*,#10711,.F.);
#15258=ORIENTED_EDGE('',*,*,#10715,.T.);
#15259=ORIENTED_EDGE('',*,*,#10703,.T.);
#15260=ORIENTED_EDGE('',*,*,#10716,.F.);
#15261=ORIENTED_EDGE('',*,*,#10684,.F.);
#15262=ORIENTED_EDGE('',*,*,#10690,.F.);
#15263=ORIENTED_EDGE('',*,*,#10713,.T.);
#15264=ORIENTED_EDGE('',*,*,#10717,.T.);
#15265=ORIENTED_EDGE('',*,*,#10707,.F.);
#15266=ORIENTED_EDGE('',*,*,#10717,.F.);
#15267=ORIENTED_EDGE('',*,*,#10712,.T.);
#15268=ORIENTED_EDGE('',*,*,#10718,.T.);
#15269=ORIENTED_EDGE('',*,*,#10706,.F.);
#15270=ORIENTED_EDGE('',*,*,#10718,.F.);
#15271=ORIENTED_EDGE('',*,*,#10704,.T.);
#15272=ORIENTED_EDGE('',*,*,#10715,.F.);
#15273=ORIENTED_EDGE('',*,*,#10710,.F.);
#15274=ORIENTED_EDGE('',*,*,#10719,.T.);
#15275=ORIENTED_EDGE('',*,*,#10587,.F.);
#15276=ORIENTED_EDGE('',*,*,#10590,.T.);
#15277=ORIENTED_EDGE('',*,*,#10720,.F.);
#15278=ORIENTED_EDGE('',*,*,#10721,.T.);
#15279=ORIENTED_EDGE('',*,*,#10722,.T.);
#15280=ORIENTED_EDGE('',*,*,#10705,.T.);
#15281=ORIENTED_EDGE('',*,*,#10719,.F.);
#15282=ORIENTED_EDGE('',*,*,#10709,.F.);
#15283=ORIENTED_EDGE('',*,*,#10723,.T.);
#15284=ORIENTED_EDGE('',*,*,#10724,.F.);
#15285=ORIENTED_EDGE('',*,*,#10702,.T.);
#15286=ORIENTED_EDGE('',*,*,#10722,.F.);
#15287=ORIENTED_EDGE('',*,*,#10725,.F.);
#15288=ORIENTED_EDGE('',*,*,#10723,.F.);
#15289=ORIENTED_EDGE('',*,*,#10708,.F.);
#15290=ORIENTED_EDGE('',*,*,#10714,.T.);
#15291=ORIENTED_EDGE('',*,*,#10701,.T.);
#15292=ORIENTED_EDGE('',*,*,#10716,.T.);
#15293=ORIENTED_EDGE('',*,*,#10726,.T.);
#15294=ORIENTED_EDGE('',*,*,#10592,.F.);
#15295=ORIENTED_EDGE('',*,*,#10727,.T.);
#15296=ORIENTED_EDGE('',*,*,#10586,.F.);
#15297=ORIENTED_EDGE('',*,*,#10728,.T.);
#15298=ORIENTED_EDGE('',*,*,#10729,.T.);
#15299=ORIENTED_EDGE('',*,*,#10726,.F.);
#15300=ORIENTED_EDGE('',*,*,#10729,.F.);
#15301=ORIENTED_EDGE('',*,*,#10730,.T.);
#15302=ORIENTED_EDGE('',*,*,#10731,.T.);
#15303=ORIENTED_EDGE('',*,*,#10727,.F.);
#15304=ORIENTED_EDGE('',*,*,#10731,.F.);
#15305=ORIENTED_EDGE('',*,*,#10724,.T.);
#15306=ORIENTED_EDGE('',*,*,#10732,.T.);
#15307=ORIENTED_EDGE('',*,*,#10733,.T.);
#15308=ORIENTED_EDGE('',*,*,#10734,.F.);
#15309=ORIENTED_EDGE('',*,*,#10735,.F.);
#15310=ORIENTED_EDGE('',*,*,#10736,.T.);
#15311=ORIENTED_EDGE('',*,*,#10720,.T.);
#15312=ORIENTED_EDGE('',*,*,#10736,.F.);
#15313=ORIENTED_EDGE('',*,*,#10737,.F.);
#15314=ORIENTED_EDGE('',*,*,#10738,.T.);
#15315=ORIENTED_EDGE('',*,*,#10739,.T.);
#15316=ORIENTED_EDGE('',*,*,#10740,.T.);
#15317=ORIENTED_EDGE('',*,*,#10721,.F.);
#15318=ORIENTED_EDGE('',*,*,#10738,.F.);
#15319=ORIENTED_EDGE('',*,*,#10741,.F.);
#15320=ORIENTED_EDGE('',*,*,#10742,.T.);
#15321=ORIENTED_EDGE('',*,*,#10743,.T.);
#15322=ORIENTED_EDGE('',*,*,#10742,.F.);
#15323=ORIENTED_EDGE('',*,*,#10744,.F.);
#15324=ORIENTED_EDGE('',*,*,#10734,.T.);
#15325=ORIENTED_EDGE('',*,*,#10744,.T.);
#15326=ORIENTED_EDGE('',*,*,#10741,.T.);
#15327=ORIENTED_EDGE('',*,*,#10737,.T.);
#15328=ORIENTED_EDGE('',*,*,#10735,.T.);
#15329=ORIENTED_EDGE('',*,*,#10728,.F.);
#15330=ORIENTED_EDGE('',*,*,#10730,.F.);
#15331=ORIENTED_EDGE('',*,*,#10745,.F.);
#15332=ORIENTED_EDGE('',*,*,#10671,.T.);
#15333=ORIENTED_EDGE('',*,*,#10746,.F.);
#15334=ORIENTED_EDGE('',*,*,#10747,.F.);
#15335=ORIENTED_EDGE('',*,*,#10748,.T.);
#15336=ORIENTED_EDGE('',*,*,#10749,.T.);
#15337=ORIENTED_EDGE('',*,*,#10750,.T.);
#15338=ORIENTED_EDGE('',*,*,#10751,.T.);
#15339=ORIENTED_EDGE('',*,*,#10752,.T.);
#15340=ORIENTED_EDGE('',*,*,#10753,.T.);
#15341=ORIENTED_EDGE('',*,*,#10754,.T.);
#15342=ORIENTED_EDGE('',*,*,#10674,.T.);
#15343=ORIENTED_EDGE('',*,*,#10755,.F.);
#15344=ORIENTED_EDGE('',*,*,#10753,.F.);
#15345=ORIENTED_EDGE('',*,*,#10756,.T.);
#15346=ORIENTED_EDGE('',*,*,#10693,.F.);
#15347=ORIENTED_EDGE('',*,*,#10698,.F.);
#15348=ORIENTED_EDGE('',*,*,#10686,.F.);
#15349=ORIENTED_EDGE('',*,*,#10757,.T.);
#15350=ORIENTED_EDGE('',*,*,#10675,.T.);
#15351=ORIENTED_EDGE('',*,*,#10754,.F.);
#15352=ORIENTED_EDGE('',*,*,#10700,.T.);
#15353=ORIENTED_EDGE('',*,*,#10756,.F.);
#15354=ORIENTED_EDGE('',*,*,#10752,.F.);
#15355=ORIENTED_EDGE('',*,*,#10758,.T.);
#15356=ORIENTED_EDGE('',*,*,#10759,.T.);
#15357=ORIENTED_EDGE('',*,*,#10584,.T.);
#15358=ORIENTED_EDGE('',*,*,#10760,.T.);
#15359=ORIENTED_EDGE('',*,*,#10659,.T.);
#15360=ORIENTED_EDGE('',*,*,#10663,.T.);
#15361=ORIENTED_EDGE('',*,*,#10667,.T.);
#15362=ORIENTED_EDGE('',*,*,#10761,.T.);
#15363=ORIENTED_EDGE('',*,*,#10648,.T.);
#15364=ORIENTED_EDGE('',*,*,#10653,.T.);
#15365=ORIENTED_EDGE('',*,*,#10656,.T.);
#15366=ORIENTED_EDGE('',*,*,#10762,.T.);
#15367=ORIENTED_EDGE('',*,*,#10746,.T.);
#15368=ORIENTED_EDGE('',*,*,#10670,.T.);
#15369=ORIENTED_EDGE('',*,*,#10676,.T.);
#15370=ORIENTED_EDGE('',*,*,#10757,.F.);
#15371=ORIENTED_EDGE('',*,*,#10739,.F.);
#15372=ORIENTED_EDGE('',*,*,#10743,.F.);
#15373=ORIENTED_EDGE('',*,*,#10733,.F.);
#15374=ORIENTED_EDGE('',*,*,#10758,.F.);
#15375=ORIENTED_EDGE('',*,*,#10751,.F.);
#15376=ORIENTED_EDGE('',*,*,#10762,.F.);
#15377=ORIENTED_EDGE('',*,*,#10655,.T.);
#15378=ORIENTED_EDGE('',*,*,#10763,.T.);
#15379=ORIENTED_EDGE('',*,*,#10747,.T.);
#15380=ORIENTED_EDGE('',*,*,#10763,.F.);
#15381=ORIENTED_EDGE('',*,*,#10657,.T.);
#15382=ORIENTED_EDGE('',*,*,#10654,.T.);
#15383=ORIENTED_EDGE('',*,*,#10651,.T.);
#15384=ORIENTED_EDGE('',*,*,#10764,.T.);
#15385=ORIENTED_EDGE('',*,*,#10677,.T.);
#15386=ORIENTED_EDGE('',*,*,#10672,.T.);
#15387=ORIENTED_EDGE('',*,*,#10745,.T.);
#15388=ORIENTED_EDGE('',*,*,#10765,.F.);
#15389=ORIENTED_EDGE('',*,*,#10665,.F.);
#15390=ORIENTED_EDGE('',*,*,#10766,.F.);
#15391=ORIENTED_EDGE('',*,*,#10748,.F.);
#15392=ORIENTED_EDGE('',*,*,#10755,.T.);
#15393=ORIENTED_EDGE('',*,*,#10673,.F.);
#15394=ORIENTED_EDGE('',*,*,#10764,.F.);
#15395=ORIENTED_EDGE('',*,*,#10650,.F.);
#15396=ORIENTED_EDGE('',*,*,#10732,.F.);
#15397=ORIENTED_EDGE('',*,*,#10725,.T.);
#15398=ORIENTED_EDGE('',*,*,#10740,.F.);
#15399=ORIENTED_EDGE('',*,*,#10759,.F.);
#15400=ORIENTED_EDGE('',*,*,#10767,.T.);
#15401=ORIENTED_EDGE('',*,*,#10660,.F.);
#15402=ORIENTED_EDGE('',*,*,#10760,.F.);
#15403=ORIENTED_EDGE('',*,*,#10750,.F.);
#15404=ORIENTED_EDGE('',*,*,#10766,.T.);
#15405=ORIENTED_EDGE('',*,*,#10668,.T.);
#15406=ORIENTED_EDGE('',*,*,#10664,.T.);
#15407=ORIENTED_EDGE('',*,*,#10661,.T.);
#15408=ORIENTED_EDGE('',*,*,#10767,.F.);
#15409=ORIENTED_EDGE('',*,*,#10749,.F.);
#15410=ORIENTED_EDGE('',*,*,#10666,.T.);
#15411=ORIENTED_EDGE('',*,*,#10765,.T.);
#15412=ORIENTED_EDGE('',*,*,#10649,.F.);
#15413=ORIENTED_EDGE('',*,*,#10761,.F.);
#15414=ORIENTED_EDGE('',*,*,#10610,.T.);
#15415=ORIENTED_EDGE('',*,*,#10608,.T.);
#15416=ORIENTED_EDGE('',*,*,#10606,.T.);
#15417=ORIENTED_EDGE('',*,*,#10604,.T.);
#15418=ORIENTED_EDGE('',*,*,#10602,.T.);
#15419=ORIENTED_EDGE('',*,*,#10599,.T.);
#15420=ORIENTED_EDGE('',*,*,#10646,.T.);
#15421=ORIENTED_EDGE('',*,*,#10644,.T.);
#15422=ORIENTED_EDGE('',*,*,#10642,.T.);
#15423=ORIENTED_EDGE('',*,*,#10640,.T.);
#15424=ORIENTED_EDGE('',*,*,#10638,.T.);
#15425=ORIENTED_EDGE('',*,*,#10636,.T.);
#15426=ORIENTED_EDGE('',*,*,#10634,.T.);
#15427=ORIENTED_EDGE('',*,*,#10632,.T.);
#15428=ORIENTED_EDGE('',*,*,#10630,.T.);
#15429=ORIENTED_EDGE('',*,*,#10628,.T.);
#15430=ORIENTED_EDGE('',*,*,#10626,.T.);
#15431=ORIENTED_EDGE('',*,*,#10623,.T.);
#15432=ORIENTED_EDGE('',*,*,#10768,.T.);
#15433=ORIENTED_EDGE('',*,*,#10769,.T.);
#15434=ORIENTED_EDGE('',*,*,#10770,.F.);
#15435=ORIENTED_EDGE('',*,*,#10771,.F.);
#15436=ORIENTED_EDGE('',*,*,#10772,.T.);
#15437=ORIENTED_EDGE('',*,*,#10769,.F.);
#15438=ORIENTED_EDGE('',*,*,#10772,.F.);
#15439=ORIENTED_EDGE('',*,*,#10768,.F.);
#15440=ORIENTED_EDGE('',*,*,#10773,.T.);
#15441=ORIENTED_EDGE('',*,*,#10770,.T.);
#15442=ORIENTED_EDGE('',*,*,#10771,.T.);
#15443=ORIENTED_EDGE('',*,*,#10773,.F.);
#15444=ORIENTED_EDGE('',*,*,#10774,.T.);
#15445=ORIENTED_EDGE('',*,*,#10775,.T.);
#15446=ORIENTED_EDGE('',*,*,#10776,.T.);
#15447=ORIENTED_EDGE('',*,*,#10777,.F.);
#15448=ORIENTED_EDGE('',*,*,#10778,.T.);
#15449=ORIENTED_EDGE('',*,*,#10779,.T.);
#15450=ORIENTED_EDGE('',*,*,#10774,.F.);
#15451=ORIENTED_EDGE('',*,*,#10780,.F.);
#15452=ORIENTED_EDGE('',*,*,#10781,.T.);
#15453=ORIENTED_EDGE('',*,*,#10782,.T.);
#15454=ORIENTED_EDGE('',*,*,#10778,.F.);
#15455=ORIENTED_EDGE('',*,*,#10783,.F.);
#15456=ORIENTED_EDGE('',*,*,#10784,.T.);
#15457=ORIENTED_EDGE('',*,*,#10785,.T.);
#15458=ORIENTED_EDGE('',*,*,#10781,.F.);
#15459=ORIENTED_EDGE('',*,*,#10786,.F.);
#15460=ORIENTED_EDGE('',*,*,#10787,.T.);
#15461=ORIENTED_EDGE('',*,*,#10788,.T.);
#15462=ORIENTED_EDGE('',*,*,#10784,.F.);
#15463=ORIENTED_EDGE('',*,*,#10789,.F.);
#15464=ORIENTED_EDGE('',*,*,#10790,.T.);
#15465=ORIENTED_EDGE('',*,*,#10791,.T.);
#15466=ORIENTED_EDGE('',*,*,#10787,.F.);
#15467=ORIENTED_EDGE('',*,*,#10792,.F.);
#15468=ORIENTED_EDGE('',*,*,#10793,.T.);
#15469=ORIENTED_EDGE('',*,*,#10794,.T.);
#15470=ORIENTED_EDGE('',*,*,#10790,.F.);
#15471=ORIENTED_EDGE('',*,*,#10795,.F.);
#15472=ORIENTED_EDGE('',*,*,#10796,.T.);
#15473=ORIENTED_EDGE('',*,*,#10797,.T.);
#15474=ORIENTED_EDGE('',*,*,#10793,.F.);
#15475=ORIENTED_EDGE('',*,*,#10798,.F.);
#15476=ORIENTED_EDGE('',*,*,#10799,.T.);
#15477=ORIENTED_EDGE('',*,*,#10800,.T.);
#15478=ORIENTED_EDGE('',*,*,#10796,.F.);
#15479=ORIENTED_EDGE('',*,*,#10801,.F.);
#15480=ORIENTED_EDGE('',*,*,#10802,.T.);
#15481=ORIENTED_EDGE('',*,*,#10803,.T.);
#15482=ORIENTED_EDGE('',*,*,#10799,.F.);
#15483=ORIENTED_EDGE('',*,*,#10804,.F.);
#15484=ORIENTED_EDGE('',*,*,#10805,.T.);
#15485=ORIENTED_EDGE('',*,*,#10806,.T.);
#15486=ORIENTED_EDGE('',*,*,#10802,.F.);
#15487=ORIENTED_EDGE('',*,*,#10807,.F.);
#15488=ORIENTED_EDGE('',*,*,#10808,.T.);
#15489=ORIENTED_EDGE('',*,*,#10809,.T.);
#15490=ORIENTED_EDGE('',*,*,#10805,.F.);
#15491=ORIENTED_EDGE('',*,*,#10810,.F.);
#15492=ORIENTED_EDGE('',*,*,#10811,.T.);
#15493=ORIENTED_EDGE('',*,*,#10812,.T.);
#15494=ORIENTED_EDGE('',*,*,#10808,.F.);
#15495=ORIENTED_EDGE('',*,*,#10813,.F.);
#15496=ORIENTED_EDGE('',*,*,#10814,.F.);
#15497=ORIENTED_EDGE('',*,*,#10815,.T.);
#15498=ORIENTED_EDGE('',*,*,#10816,.T.);
#15499=ORIENTED_EDGE('',*,*,#10817,.T.);
#15500=ORIENTED_EDGE('',*,*,#10818,.T.);
#15501=ORIENTED_EDGE('',*,*,#10819,.T.);
#15502=ORIENTED_EDGE('',*,*,#10820,.F.);
#15503=ORIENTED_EDGE('',*,*,#10821,.T.);
#15504=ORIENTED_EDGE('',*,*,#10822,.T.);
#15505=ORIENTED_EDGE('',*,*,#10817,.F.);
#15506=ORIENTED_EDGE('',*,*,#10823,.F.);
#15507=ORIENTED_EDGE('',*,*,#10824,.T.);
#15508=ORIENTED_EDGE('',*,*,#10825,.T.);
#15509=ORIENTED_EDGE('',*,*,#10821,.F.);
#15510=ORIENTED_EDGE('',*,*,#10826,.F.);
#15511=ORIENTED_EDGE('',*,*,#10827,.T.);
#15512=ORIENTED_EDGE('',*,*,#10828,.T.);
#15513=ORIENTED_EDGE('',*,*,#10824,.F.);
#15514=ORIENTED_EDGE('',*,*,#10829,.F.);
#15515=ORIENTED_EDGE('',*,*,#10830,.T.);
#15516=ORIENTED_EDGE('',*,*,#10831,.T.);
#15517=ORIENTED_EDGE('',*,*,#10827,.F.);
#15518=ORIENTED_EDGE('',*,*,#10832,.F.);
#15519=ORIENTED_EDGE('',*,*,#10833,.T.);
#15520=ORIENTED_EDGE('',*,*,#10834,.T.);
#15521=ORIENTED_EDGE('',*,*,#10830,.F.);
#15522=ORIENTED_EDGE('',*,*,#10835,.F.);
#15523=ORIENTED_EDGE('',*,*,#10836,.T.);
#15524=ORIENTED_EDGE('',*,*,#10837,.T.);
#15525=ORIENTED_EDGE('',*,*,#10833,.F.);
#15526=ORIENTED_EDGE('',*,*,#10838,.F.);
#15527=ORIENTED_EDGE('',*,*,#10839,.T.);
#15528=ORIENTED_EDGE('',*,*,#10840,.T.);
#15529=ORIENTED_EDGE('',*,*,#10836,.F.);
#15530=ORIENTED_EDGE('',*,*,#10841,.F.);
#15531=ORIENTED_EDGE('',*,*,#10842,.T.);
#15532=ORIENTED_EDGE('',*,*,#10843,.T.);
#15533=ORIENTED_EDGE('',*,*,#10839,.F.);
#15534=ORIENTED_EDGE('',*,*,#10844,.F.);
#15535=ORIENTED_EDGE('',*,*,#10845,.T.);
#15536=ORIENTED_EDGE('',*,*,#10846,.T.);
#15537=ORIENTED_EDGE('',*,*,#10842,.F.);
#15538=ORIENTED_EDGE('',*,*,#10847,.F.);
#15539=ORIENTED_EDGE('',*,*,#10848,.T.);
#15540=ORIENTED_EDGE('',*,*,#10849,.T.);
#15541=ORIENTED_EDGE('',*,*,#10845,.F.);
#15542=ORIENTED_EDGE('',*,*,#10850,.F.);
#15543=ORIENTED_EDGE('',*,*,#10851,.T.);
#15544=ORIENTED_EDGE('',*,*,#10852,.T.);
#15545=ORIENTED_EDGE('',*,*,#10848,.F.);
#15546=ORIENTED_EDGE('',*,*,#10853,.F.);
#15547=ORIENTED_EDGE('',*,*,#10854,.T.);
#15548=ORIENTED_EDGE('',*,*,#10855,.T.);
#15549=ORIENTED_EDGE('',*,*,#10851,.F.);
#15550=ORIENTED_EDGE('',*,*,#10856,.F.);
#15551=ORIENTED_EDGE('',*,*,#10857,.F.);
#15552=ORIENTED_EDGE('',*,*,#10858,.F.);
#15553=ORIENTED_EDGE('',*,*,#10859,.T.);
#15554=ORIENTED_EDGE('',*,*,#10860,.T.);
#15555=ORIENTED_EDGE('',*,*,#10861,.F.);
#15556=ORIENTED_EDGE('',*,*,#10862,.T.);
#15557=ORIENTED_EDGE('',*,*,#10863,.T.);
#15558=ORIENTED_EDGE('',*,*,#10862,.F.);
#15559=ORIENTED_EDGE('',*,*,#10864,.T.);
#15560=ORIENTED_EDGE('',*,*,#10865,.T.);
#15561=ORIENTED_EDGE('',*,*,#10866,.T.);
#15562=ORIENTED_EDGE('',*,*,#10865,.F.);
#15563=ORIENTED_EDGE('',*,*,#10867,.T.);
#15564=ORIENTED_EDGE('',*,*,#10868,.T.);
#15565=ORIENTED_EDGE('',*,*,#10869,.T.);
#15566=ORIENTED_EDGE('',*,*,#10868,.F.);
#15567=ORIENTED_EDGE('',*,*,#10870,.F.);
#15568=ORIENTED_EDGE('',*,*,#10871,.T.);
#15569=ORIENTED_EDGE('',*,*,#10872,.F.);
#15570=ORIENTED_EDGE('',*,*,#10873,.F.);
#15571=ORIENTED_EDGE('',*,*,#10871,.F.);
#15572=ORIENTED_EDGE('',*,*,#10874,.F.);
#15573=ORIENTED_EDGE('',*,*,#10875,.F.);
#15574=ORIENTED_EDGE('',*,*,#10876,.T.);
#15575=ORIENTED_EDGE('',*,*,#10877,.F.);
#15576=ORIENTED_EDGE('',*,*,#10876,.F.);
#15577=ORIENTED_EDGE('',*,*,#10878,.F.);
#15578=ORIENTED_EDGE('',*,*,#10879,.F.);
#15579=ORIENTED_EDGE('',*,*,#10880,.T.);
#15580=ORIENTED_EDGE('',*,*,#10881,.F.);
#15581=ORIENTED_EDGE('',*,*,#10880,.F.);
#15582=ORIENTED_EDGE('',*,*,#10882,.F.);
#15583=ORIENTED_EDGE('',*,*,#10883,.T.);
#15584=ORIENTED_EDGE('',*,*,#10884,.F.);
#15585=ORIENTED_EDGE('',*,*,#10885,.F.);
#15586=ORIENTED_EDGE('',*,*,#10883,.F.);
#15587=ORIENTED_EDGE('',*,*,#10878,.T.);
#15588=ORIENTED_EDGE('',*,*,#10879,.T.);
#15589=ORIENTED_EDGE('',*,*,#10886,.T.);
#15590=ORIENTED_EDGE('',*,*,#10884,.T.);
#15591=ORIENTED_EDGE('',*,*,#10885,.T.);
#15592=ORIENTED_EDGE('',*,*,#10886,.F.);
#15593=ORIENTED_EDGE('',*,*,#10874,.T.);
#15594=ORIENTED_EDGE('',*,*,#10875,.T.);
#15595=ORIENTED_EDGE('',*,*,#10887,.T.);
#15596=ORIENTED_EDGE('',*,*,#10872,.T.);
#15597=ORIENTED_EDGE('',*,*,#10873,.T.);
#15598=ORIENTED_EDGE('',*,*,#10887,.F.);
#15599=ORIENTED_EDGE('',*,*,#10877,.T.);
#15600=ORIENTED_EDGE('',*,*,#10882,.T.);
#15601=ORIENTED_EDGE('',*,*,#10870,.T.);
#15602=ORIENTED_EDGE('',*,*,#10888,.F.);
#15603=ORIENTED_EDGE('',*,*,#10881,.T.);
#15604=ORIENTED_EDGE('',*,*,#10889,.T.);
#15605=ORIENTED_EDGE('',*,*,#10890,.T.);
#15606=ORIENTED_EDGE('',*,*,#10891,.T.);
#15607=ORIENTED_EDGE('',*,*,#10892,.T.);
#15608=ORIENTED_EDGE('',*,*,#10893,.T.);
#15609=ORIENTED_EDGE('',*,*,#10894,.T.);
#15610=ORIENTED_EDGE('',*,*,#10858,.T.);
#15611=ORIENTED_EDGE('',*,*,#10895,.T.);
#15612=ORIENTED_EDGE('',*,*,#10856,.T.);
#15613=ORIENTED_EDGE('',*,*,#10853,.T.);
#15614=ORIENTED_EDGE('',*,*,#10850,.T.);
#15615=ORIENTED_EDGE('',*,*,#10847,.T.);
#15616=ORIENTED_EDGE('',*,*,#10844,.T.);
#15617=ORIENTED_EDGE('',*,*,#10841,.T.);
#15618=ORIENTED_EDGE('',*,*,#10838,.T.);
#15619=ORIENTED_EDGE('',*,*,#10835,.T.);
#15620=ORIENTED_EDGE('',*,*,#10832,.T.);
#15621=ORIENTED_EDGE('',*,*,#10829,.T.);
#15622=ORIENTED_EDGE('',*,*,#10826,.T.);
#15623=ORIENTED_EDGE('',*,*,#10823,.T.);
#15624=ORIENTED_EDGE('',*,*,#10820,.T.);
#15625=ORIENTED_EDGE('',*,*,#10896,.T.);
#15626=ORIENTED_EDGE('',*,*,#10779,.F.);
#15627=ORIENTED_EDGE('',*,*,#10782,.F.);
#15628=ORIENTED_EDGE('',*,*,#10785,.F.);
#15629=ORIENTED_EDGE('',*,*,#10788,.F.);
#15630=ORIENTED_EDGE('',*,*,#10791,.F.);
#15631=ORIENTED_EDGE('',*,*,#10794,.F.);
#15632=ORIENTED_EDGE('',*,*,#10797,.F.);
#15633=ORIENTED_EDGE('',*,*,#10800,.F.);
#15634=ORIENTED_EDGE('',*,*,#10803,.F.);
#15635=ORIENTED_EDGE('',*,*,#10806,.F.);
#15636=ORIENTED_EDGE('',*,*,#10809,.F.);
#15637=ORIENTED_EDGE('',*,*,#10812,.F.);
#15638=ORIENTED_EDGE('',*,*,#10897,.F.);
#15639=ORIENTED_EDGE('',*,*,#10816,.F.);
#15640=ORIENTED_EDGE('',*,*,#10890,.F.);
#15641=ORIENTED_EDGE('',*,*,#10857,.T.);
#15642=ORIENTED_EDGE('',*,*,#10898,.T.);
#15643=ORIENTED_EDGE('',*,*,#10854,.F.);
#15644=ORIENTED_EDGE('',*,*,#10895,.F.);
#15645=ORIENTED_EDGE('',*,*,#10899,.T.);
#15646=ORIENTED_EDGE('',*,*,#10900,.T.);
#15647=ORIENTED_EDGE('',*,*,#10813,.T.);
#15648=ORIENTED_EDGE('',*,*,#10810,.T.);
#15649=ORIENTED_EDGE('',*,*,#10807,.T.);
#15650=ORIENTED_EDGE('',*,*,#10804,.T.);
#15651=ORIENTED_EDGE('',*,*,#10801,.T.);
#15652=ORIENTED_EDGE('',*,*,#10798,.T.);
#15653=ORIENTED_EDGE('',*,*,#10795,.T.);
#15654=ORIENTED_EDGE('',*,*,#10792,.T.);
#15655=ORIENTED_EDGE('',*,*,#10789,.T.);
#15656=ORIENTED_EDGE('',*,*,#10786,.T.);
#15657=ORIENTED_EDGE('',*,*,#10783,.T.);
#15658=ORIENTED_EDGE('',*,*,#10780,.T.);
#15659=ORIENTED_EDGE('',*,*,#10777,.T.);
#15660=ORIENTED_EDGE('',*,*,#10901,.T.);
#15661=ORIENTED_EDGE('',*,*,#10902,.T.);
#15662=ORIENTED_EDGE('',*,*,#10818,.F.);
#15663=ORIENTED_EDGE('',*,*,#10822,.F.);
#15664=ORIENTED_EDGE('',*,*,#10825,.F.);
#15665=ORIENTED_EDGE('',*,*,#10828,.F.);
#15666=ORIENTED_EDGE('',*,*,#10831,.F.);
#15667=ORIENTED_EDGE('',*,*,#10834,.F.);
#15668=ORIENTED_EDGE('',*,*,#10837,.F.);
#15669=ORIENTED_EDGE('',*,*,#10840,.F.);
#15670=ORIENTED_EDGE('',*,*,#10843,.F.);
#15671=ORIENTED_EDGE('',*,*,#10846,.F.);
#15672=ORIENTED_EDGE('',*,*,#10849,.F.);
#15673=ORIENTED_EDGE('',*,*,#10852,.F.);
#15674=ORIENTED_EDGE('',*,*,#10855,.F.);
#15675=ORIENTED_EDGE('',*,*,#10898,.F.);
#15676=ORIENTED_EDGE('',*,*,#10860,.F.);
#15677=ORIENTED_EDGE('',*,*,#10902,.F.);
#15678=ORIENTED_EDGE('',*,*,#10903,.F.);
#15679=ORIENTED_EDGE('',*,*,#10775,.F.);
#15680=ORIENTED_EDGE('',*,*,#10896,.F.);
#15681=ORIENTED_EDGE('',*,*,#10819,.F.);
#15682=ORIENTED_EDGE('',*,*,#10899,.F.);
#15683=ORIENTED_EDGE('',*,*,#10859,.F.);
#15684=ORIENTED_EDGE('',*,*,#10894,.F.);
#15685=ORIENTED_EDGE('',*,*,#10893,.F.);
#15686=ORIENTED_EDGE('',*,*,#10901,.F.);
#15687=ORIENTED_EDGE('',*,*,#10904,.T.);
#15688=ORIENTED_EDGE('',*,*,#10903,.T.);
#15689=ORIENTED_EDGE('',*,*,#10891,.F.);
#15690=ORIENTED_EDGE('',*,*,#10815,.F.);
#15691=ORIENTED_EDGE('',*,*,#10892,.F.);
#15692=ORIENTED_EDGE('',*,*,#10905,.T.);
#15693=ORIENTED_EDGE('',*,*,#10906,.F.);
#15694=ORIENTED_EDGE('',*,*,#10905,.F.);
#15695=ORIENTED_EDGE('',*,*,#10776,.F.);
#15696=ORIENTED_EDGE('',*,*,#10907,.T.);
#15697=ORIENTED_EDGE('',*,*,#10889,.F.);
#15698=ORIENTED_EDGE('',*,*,#10907,.F.);
#15699=ORIENTED_EDGE('',*,*,#10904,.F.);
#15700=ORIENTED_EDGE('',*,*,#10908,.F.);
#15701=ORIENTED_EDGE('',*,*,#10909,.F.);
#15702=ORIENTED_EDGE('',*,*,#10910,.T.);
#15703=ORIENTED_EDGE('',*,*,#10911,.F.);
#15704=ORIENTED_EDGE('',*,*,#10910,.F.);
#15705=ORIENTED_EDGE('',*,*,#10911,.T.);
#15706=ORIENTED_EDGE('',*,*,#10906,.T.);
#15707=ORIENTED_EDGE('',*,*,#10814,.T.);
#15708=ORIENTED_EDGE('',*,*,#10897,.T.);
#15709=ORIENTED_EDGE('',*,*,#10811,.F.);
#15710=ORIENTED_EDGE('',*,*,#10900,.F.);
#15711=ORIENTED_EDGE('',*,*,#10866,.F.);
#15712=ORIENTED_EDGE('',*,*,#10912,.F.);
#15713=ORIENTED_EDGE('',*,*,#10913,.T.);
#15714=ORIENTED_EDGE('',*,*,#10914,.F.);
#15715=ORIENTED_EDGE('',*,*,#10913,.F.);
#15716=ORIENTED_EDGE('',*,*,#10915,.F.);
#15717=ORIENTED_EDGE('',*,*,#10916,.T.);
#15718=ORIENTED_EDGE('',*,*,#10917,.F.);
#15719=ORIENTED_EDGE('',*,*,#10916,.F.);
#15720=ORIENTED_EDGE('',*,*,#10917,.T.);
#15721=ORIENTED_EDGE('',*,*,#10918,.T.);
#15722=ORIENTED_EDGE('',*,*,#10912,.T.);
#15723=ORIENTED_EDGE('',*,*,#10918,.F.);
#15724=ORIENTED_EDGE('',*,*,#10919,.T.);
#15725=ORIENTED_EDGE('',*,*,#10920,.T.);
#15726=ORIENTED_EDGE('',*,*,#10888,.T.);
#15727=ORIENTED_EDGE('',*,*,#10920,.F.);
#15728=ORIENTED_EDGE('',*,*,#10921,.F.);
#15729=ORIENTED_EDGE('',*,*,#10922,.T.);
#15730=ORIENTED_EDGE('',*,*,#10923,.F.);
#15731=ORIENTED_EDGE('',*,*,#10924,.F.);
#15732=ORIENTED_EDGE('',*,*,#10925,.T.);
#15733=ORIENTED_EDGE('',*,*,#10926,.T.);
#15734=ORIENTED_EDGE('',*,*,#10927,.T.);
#15735=ORIENTED_EDGE('',*,*,#10926,.F.);
#15736=ORIENTED_EDGE('',*,*,#10928,.T.);
#15737=ORIENTED_EDGE('',*,*,#10929,.T.);
#15738=ORIENTED_EDGE('',*,*,#10930,.T.);
#15739=ORIENTED_EDGE('',*,*,#10931,.T.);
#15740=ORIENTED_EDGE('',*,*,#10932,.T.);
#15741=ORIENTED_EDGE('',*,*,#10933,.T.);
#15742=ORIENTED_EDGE('',*,*,#10934,.T.);
#15743=ORIENTED_EDGE('',*,*,#10935,.T.);
#15744=ORIENTED_EDGE('',*,*,#10936,.T.);
#15745=ORIENTED_EDGE('',*,*,#10937,.T.);
#15746=ORIENTED_EDGE('',*,*,#10938,.T.);
#15747=ORIENTED_EDGE('',*,*,#10939,.T.);
#15748=ORIENTED_EDGE('',*,*,#10940,.T.);
#15749=ORIENTED_EDGE('',*,*,#10941,.T.);
#15750=ORIENTED_EDGE('',*,*,#10919,.F.);
#15751=ORIENTED_EDGE('',*,*,#10927,.F.);
#15752=ORIENTED_EDGE('',*,*,#10942,.F.);
#15753=ORIENTED_EDGE('',*,*,#10943,.T.);
#15754=ORIENTED_EDGE('',*,*,#10944,.F.);
#15755=ORIENTED_EDGE('',*,*,#10945,.F.);
#15756=ORIENTED_EDGE('',*,*,#10946,.F.);
#15757=ORIENTED_EDGE('',*,*,#10947,.T.);
#15758=ORIENTED_EDGE('',*,*,#10948,.F.);
#15759=ORIENTED_EDGE('',*,*,#10949,.F.);
#15760=ORIENTED_EDGE('',*,*,#10950,.T.);
#15761=ORIENTED_EDGE('',*,*,#10951,.F.);
#15762=ORIENTED_EDGE('',*,*,#10952,.F.);
#15763=ORIENTED_EDGE('',*,*,#10953,.F.);
#15764=ORIENTED_EDGE('',*,*,#10954,.F.);
#15765=ORIENTED_EDGE('',*,*,#10955,.F.);
#15766=ORIENTED_EDGE('',*,*,#10956,.F.);
#15767=ORIENTED_EDGE('',*,*,#10957,.F.);
#15768=ORIENTED_EDGE('',*,*,#10958,.F.);
#15769=ORIENTED_EDGE('',*,*,#10959,.F.);
#15770=ORIENTED_EDGE('',*,*,#10960,.T.);
#15771=ORIENTED_EDGE('',*,*,#10961,.F.);
#15772=ORIENTED_EDGE('',*,*,#10962,.F.);
#15773=ORIENTED_EDGE('',*,*,#10963,.F.);
#15774=ORIENTED_EDGE('',*,*,#10964,.F.);
#15775=ORIENTED_EDGE('',*,*,#10965,.F.);
#15776=ORIENTED_EDGE('',*,*,#10966,.F.);
#15777=ORIENTED_EDGE('',*,*,#10967,.F.);
#15778=ORIENTED_EDGE('',*,*,#10968,.T.);
#15779=ORIENTED_EDGE('',*,*,#10969,.T.);
#15780=ORIENTED_EDGE('',*,*,#10970,.T.);
#15781=ORIENTED_EDGE('',*,*,#10946,.T.);
#15782=ORIENTED_EDGE('',*,*,#10971,.F.);
#15783=ORIENTED_EDGE('',*,*,#10930,.F.);
#15784=ORIENTED_EDGE('',*,*,#10972,.T.);
#15785=ORIENTED_EDGE('',*,*,#10973,.F.);
#15786=ORIENTED_EDGE('',*,*,#10974,.T.);
#15787=ORIENTED_EDGE('',*,*,#10975,.F.);
#15788=ORIENTED_EDGE('',*,*,#10945,.T.);
#15789=ORIENTED_EDGE('',*,*,#10959,.T.);
#15790=ORIENTED_EDGE('',*,*,#10976,.F.);
#15791=ORIENTED_EDGE('',*,*,#10931,.F.);
#15792=ORIENTED_EDGE('',*,*,#10971,.T.);
#15793=ORIENTED_EDGE('',*,*,#10958,.T.);
#15794=ORIENTED_EDGE('',*,*,#10977,.F.);
#15795=ORIENTED_EDGE('',*,*,#10932,.F.);
#15796=ORIENTED_EDGE('',*,*,#10976,.T.);
#15797=ORIENTED_EDGE('',*,*,#10957,.T.);
#15798=ORIENTED_EDGE('',*,*,#10978,.F.);
#15799=ORIENTED_EDGE('',*,*,#10933,.F.);
#15800=ORIENTED_EDGE('',*,*,#10977,.T.);
#15801=ORIENTED_EDGE('',*,*,#10956,.T.);
#15802=ORIENTED_EDGE('',*,*,#10979,.F.);
#15803=ORIENTED_EDGE('',*,*,#10934,.F.);
#15804=ORIENTED_EDGE('',*,*,#10978,.T.);
#15805=ORIENTED_EDGE('',*,*,#10955,.T.);
#15806=ORIENTED_EDGE('',*,*,#10980,.F.);
#15807=ORIENTED_EDGE('',*,*,#10935,.F.);
#15808=ORIENTED_EDGE('',*,*,#10979,.T.);
#15809=ORIENTED_EDGE('',*,*,#10954,.T.);
#15810=ORIENTED_EDGE('',*,*,#10981,.F.);
#15811=ORIENTED_EDGE('',*,*,#10936,.F.);
#15812=ORIENTED_EDGE('',*,*,#10980,.T.);
#15813=ORIENTED_EDGE('',*,*,#10953,.T.);
#15814=ORIENTED_EDGE('',*,*,#10982,.F.);
#15815=ORIENTED_EDGE('',*,*,#10937,.F.);
#15816=ORIENTED_EDGE('',*,*,#10981,.T.);
#15817=ORIENTED_EDGE('',*,*,#10952,.T.);
#15818=ORIENTED_EDGE('',*,*,#10983,.F.);
#15819=ORIENTED_EDGE('',*,*,#10938,.F.);
#15820=ORIENTED_EDGE('',*,*,#10982,.T.);
#15821=ORIENTED_EDGE('',*,*,#10951,.T.);
#15822=ORIENTED_EDGE('',*,*,#10984,.T.);
#15823=ORIENTED_EDGE('',*,*,#10985,.F.);
#15824=ORIENTED_EDGE('',*,*,#10986,.T.);
#15825=ORIENTED_EDGE('',*,*,#10987,.F.);
#15826=ORIENTED_EDGE('',*,*,#10922,.F.);
#15827=ORIENTED_EDGE('',*,*,#10988,.F.);
#15828=ORIENTED_EDGE('',*,*,#10989,.T.);
#15829=ORIENTED_EDGE('',*,*,#10990,.T.);
#15830=ORIENTED_EDGE('',*,*,#10991,.T.);
#15831=ORIENTED_EDGE('',*,*,#10939,.F.);
#15832=ORIENTED_EDGE('',*,*,#10983,.T.);
#15833=ORIENTED_EDGE('',*,*,#10992,.T.);
#15834=ORIENTED_EDGE('',*,*,#10993,.T.);
#15835=ORIENTED_EDGE('',*,*,#10949,.T.);
#15836=ORIENTED_EDGE('',*,*,#10994,.F.);
#15837=ORIENTED_EDGE('',*,*,#10941,.F.);
#15838=ORIENTED_EDGE('',*,*,#10995,.T.);
#15839=ORIENTED_EDGE('',*,*,#10996,.F.);
#15840=ORIENTED_EDGE('',*,*,#10997,.T.);
#15841=ORIENTED_EDGE('',*,*,#10998,.F.);
#15842=ORIENTED_EDGE('',*,*,#10924,.T.);
#15843=ORIENTED_EDGE('',*,*,#10999,.F.);
#15844=ORIENTED_EDGE('',*,*,#11000,.T.);
#15845=ORIENTED_EDGE('',*,*,#11001,.F.);
#15846=ORIENTED_EDGE('',*,*,#11002,.T.);
#15847=ORIENTED_EDGE('',*,*,#11003,.F.);
#15848=ORIENTED_EDGE('',*,*,#10943,.F.);
#15849=ORIENTED_EDGE('',*,*,#11004,.F.);
#15850=ORIENTED_EDGE('',*,*,#11005,.T.);
#15851=ORIENTED_EDGE('',*,*,#11006,.T.);
#15852=ORIENTED_EDGE('',*,*,#11007,.T.);
#15853=ORIENTED_EDGE('',*,*,#10928,.F.);
#15854=ORIENTED_EDGE('',*,*,#10994,.T.);
#15855=ORIENTED_EDGE('',*,*,#10948,.T.);
#15856=ORIENTED_EDGE('',*,*,#11008,.T.);
#15857=ORIENTED_EDGE('',*,*,#10998,.T.);
#15858=ORIENTED_EDGE('',*,*,#11009,.T.);
#15859=ORIENTED_EDGE('',*,*,#10988,.T.);
#15860=ORIENTED_EDGE('',*,*,#10921,.T.);
#15861=ORIENTED_EDGE('',*,*,#10996,.T.);
#15862=ORIENTED_EDGE('',*,*,#11010,.T.);
#15863=ORIENTED_EDGE('',*,*,#10990,.F.);
#15864=ORIENTED_EDGE('',*,*,#11011,.T.);
#15865=ORIENTED_EDGE('',*,*,#10992,.F.);
#15866=ORIENTED_EDGE('',*,*,#11012,.T.);
#15867=ORIENTED_EDGE('',*,*,#10985,.T.);
#15868=ORIENTED_EDGE('',*,*,#11013,.T.);
#15869=ORIENTED_EDGE('',*,*,#10987,.T.);
#15870=ORIENTED_EDGE('',*,*,#11014,.T.);
#15871=ORIENTED_EDGE('',*,*,#10999,.T.);
#15872=ORIENTED_EDGE('',*,*,#10923,.T.);
#15873=ORIENTED_EDGE('',*,*,#10867,.F.);
#15874=ORIENTED_EDGE('',*,*,#10986,.F.);
#15875=ORIENTED_EDGE('',*,*,#11012,.F.);
#15876=ORIENTED_EDGE('',*,*,#11000,.F.);
#15877=ORIENTED_EDGE('',*,*,#11014,.F.);
#15878=ORIENTED_EDGE('',*,*,#10984,.F.);
#15879=ORIENTED_EDGE('',*,*,#10950,.F.);
#15880=ORIENTED_EDGE('',*,*,#10993,.F.);
#15881=ORIENTED_EDGE('',*,*,#11013,.F.);
#15882=ORIENTED_EDGE('',*,*,#10995,.F.);
#15883=ORIENTED_EDGE('',*,*,#10940,.F.);
#15884=ORIENTED_EDGE('',*,*,#10991,.F.);
#15885=ORIENTED_EDGE('',*,*,#11010,.F.);
#15886=ORIENTED_EDGE('',*,*,#10997,.F.);
#15887=ORIENTED_EDGE('',*,*,#11011,.F.);
#15888=ORIENTED_EDGE('',*,*,#10989,.F.);
#15889=ORIENTED_EDGE('',*,*,#11009,.F.);
#15890=ORIENTED_EDGE('',*,*,#11003,.T.);
#15891=ORIENTED_EDGE('',*,*,#11015,.T.);
#15892=ORIENTED_EDGE('',*,*,#10967,.T.);
#15893=ORIENTED_EDGE('',*,*,#10944,.T.);
#15894=ORIENTED_EDGE('',*,*,#10969,.F.);
#15895=ORIENTED_EDGE('',*,*,#11016,.T.);
#15896=ORIENTED_EDGE('',*,*,#11001,.T.);
#15897=ORIENTED_EDGE('',*,*,#11017,.T.);
#15898=ORIENTED_EDGE('',*,*,#11006,.F.);
#15899=ORIENTED_EDGE('',*,*,#11018,.T.);
#15900=ORIENTED_EDGE('',*,*,#10973,.T.);
#15901=ORIENTED_EDGE('',*,*,#11019,.T.);
#15902=ORIENTED_EDGE('',*,*,#10975,.T.);
#15903=ORIENTED_EDGE('',*,*,#11020,.T.);
#15904=ORIENTED_EDGE('',*,*,#11004,.T.);
#15905=ORIENTED_EDGE('',*,*,#10942,.T.);
#15906=ORIENTED_EDGE('',*,*,#10864,.F.);
#15907=ORIENTED_EDGE('',*,*,#11002,.F.);
#15908=ORIENTED_EDGE('',*,*,#11016,.F.);
#15909=ORIENTED_EDGE('',*,*,#10968,.F.);
#15910=ORIENTED_EDGE('',*,*,#11015,.F.);
#15911=ORIENTED_EDGE('',*,*,#11008,.F.);
#15912=ORIENTED_EDGE('',*,*,#10947,.F.);
#15913=ORIENTED_EDGE('',*,*,#10970,.F.);
#15914=ORIENTED_EDGE('',*,*,#11017,.F.);
#15915=ORIENTED_EDGE('',*,*,#10974,.F.);
#15916=ORIENTED_EDGE('',*,*,#11018,.F.);
#15917=ORIENTED_EDGE('',*,*,#11005,.F.);
#15918=ORIENTED_EDGE('',*,*,#11020,.F.);
#15919=ORIENTED_EDGE('',*,*,#10972,.F.);
#15920=ORIENTED_EDGE('',*,*,#10929,.F.);
#15921=ORIENTED_EDGE('',*,*,#11007,.F.);
#15922=ORIENTED_EDGE('',*,*,#11019,.F.);
#15923=ORIENTED_EDGE('',*,*,#10914,.T.);
#15924=ORIENTED_EDGE('',*,*,#10925,.F.);
#15925=ORIENTED_EDGE('',*,*,#10915,.T.);
#15926=ORIENTED_EDGE('',*,*,#11021,.T.);
#15927=ORIENTED_EDGE('',*,*,#11022,.T.);
#15928=ORIENTED_EDGE('',*,*,#11023,.F.);
#15929=ORIENTED_EDGE('',*,*,#10962,.T.);
#15930=ORIENTED_EDGE('',*,*,#11024,.T.);
#15931=ORIENTED_EDGE('',*,*,#11025,.T.);
#15932=ORIENTED_EDGE('',*,*,#11021,.F.);
#15933=ORIENTED_EDGE('',*,*,#10961,.T.);
#15934=ORIENTED_EDGE('',*,*,#11026,.T.);
#15935=ORIENTED_EDGE('',*,*,#11027,.T.);
#15936=ORIENTED_EDGE('',*,*,#11024,.F.);
#15937=ORIENTED_EDGE('',*,*,#10966,.T.);
#15938=ORIENTED_EDGE('',*,*,#11028,.T.);
#15939=ORIENTED_EDGE('',*,*,#11029,.T.);
#15940=ORIENTED_EDGE('',*,*,#11026,.F.);
#15941=ORIENTED_EDGE('',*,*,#10965,.T.);
#15942=ORIENTED_EDGE('',*,*,#11030,.T.);
#15943=ORIENTED_EDGE('',*,*,#11031,.T.);
#15944=ORIENTED_EDGE('',*,*,#11028,.F.);
#15945=ORIENTED_EDGE('',*,*,#10964,.T.);
#15946=ORIENTED_EDGE('',*,*,#11023,.T.);
#15947=ORIENTED_EDGE('',*,*,#11032,.T.);
#15948=ORIENTED_EDGE('',*,*,#11030,.F.);
#15949=ORIENTED_EDGE('',*,*,#10963,.T.);
#15950=ORIENTED_EDGE('',*,*,#11033,.T.);
#15951=ORIENTED_EDGE('',*,*,#11034,.T.);
#15952=ORIENTED_EDGE('',*,*,#11035,.T.);
#15953=ORIENTED_EDGE('',*,*,#11036,.T.);
#15954=ORIENTED_EDGE('',*,*,#11037,.T.);
#15955=ORIENTED_EDGE('',*,*,#11038,.T.);
#15956=ORIENTED_EDGE('',*,*,#11039,.F.);
#15957=ORIENTED_EDGE('',*,*,#11025,.F.);
#15958=ORIENTED_EDGE('',*,*,#11040,.F.);
#15959=ORIENTED_EDGE('',*,*,#11037,.F.);
#15960=ORIENTED_EDGE('',*,*,#11040,.T.);
#15961=ORIENTED_EDGE('',*,*,#11027,.F.);
#15962=ORIENTED_EDGE('',*,*,#11041,.F.);
#15963=ORIENTED_EDGE('',*,*,#11038,.F.);
#15964=ORIENTED_EDGE('',*,*,#11039,.T.);
#15965=ORIENTED_EDGE('',*,*,#11036,.F.);
#15966=ORIENTED_EDGE('',*,*,#11042,.F.);
#15967=ORIENTED_EDGE('',*,*,#11022,.F.);
#15968=ORIENTED_EDGE('',*,*,#11041,.T.);
#15969=ORIENTED_EDGE('',*,*,#11029,.F.);
#15970=ORIENTED_EDGE('',*,*,#11043,.F.);
#15971=ORIENTED_EDGE('',*,*,#11033,.F.);
#15972=ORIENTED_EDGE('',*,*,#11042,.T.);
#15973=ORIENTED_EDGE('',*,*,#11035,.F.);
#15974=ORIENTED_EDGE('',*,*,#11044,.F.);
#15975=ORIENTED_EDGE('',*,*,#11032,.F.);
#15976=ORIENTED_EDGE('',*,*,#11043,.T.);
#15977=ORIENTED_EDGE('',*,*,#11031,.F.);
#15978=ORIENTED_EDGE('',*,*,#11044,.T.);
#15979=ORIENTED_EDGE('',*,*,#11034,.F.);
#15980=ORIENTED_EDGE('',*,*,#10908,.T.);
#15981=ORIENTED_EDGE('',*,*,#10909,.T.);
#15982=ORIENTED_EDGE('',*,*,#11045,.T.);
#15983=ORIENTED_EDGE('',*,*,#10960,.F.);
#15984=ORIENTED_EDGE('',*,*,#11045,.F.);
#15985=ORIENTED_EDGE('',*,*,#11046,.F.);
#15986=ORIENTED_EDGE('',*,*,#10869,.F.);
#15987=ORIENTED_EDGE('',*,*,#11046,.T.);
#15988=ORIENTED_EDGE('',*,*,#11047,.T.);
#15989=ORIENTED_EDGE('',*,*,#11048,.F.);
#15990=ORIENTED_EDGE('',*,*,#11047,.F.);
#15991=ORIENTED_EDGE('',*,*,#11049,.T.);
#15992=ORIENTED_EDGE('',*,*,#11050,.F.);
#15993=ORIENTED_EDGE('',*,*,#11051,.F.);
#15994=ORIENTED_EDGE('',*,*,#11052,.T.);
#15995=ORIENTED_EDGE('',*,*,#11053,.F.);
#15996=ORIENTED_EDGE('',*,*,#11054,.T.);
#15997=ORIENTED_EDGE('',*,*,#11055,.T.);
#15998=ORIENTED_EDGE('',*,*,#11052,.F.);
#15999=ORIENTED_EDGE('',*,*,#11056,.T.);
#16000=ORIENTED_EDGE('',*,*,#11054,.F.);
#16001=ORIENTED_EDGE('',*,*,#11057,.F.);
#16002=ORIENTED_EDGE('',*,*,#11058,.T.);
#16003=ORIENTED_EDGE('',*,*,#11059,.T.);
#16004=ORIENTED_EDGE('',*,*,#11058,.F.);
#16005=ORIENTED_EDGE('',*,*,#11060,.F.);
#16006=ORIENTED_EDGE('',*,*,#11061,.T.);
#16007=ORIENTED_EDGE('',*,*,#11062,.T.);
#16008=ORIENTED_EDGE('',*,*,#11061,.F.);
#16009=ORIENTED_EDGE('',*,*,#11063,.F.);
#16010=ORIENTED_EDGE('',*,*,#11064,.T.);
#16011=ORIENTED_EDGE('',*,*,#11065,.T.);
#16012=ORIENTED_EDGE('',*,*,#11064,.F.);
#16013=ORIENTED_EDGE('',*,*,#11066,.F.);
#16014=ORIENTED_EDGE('',*,*,#11067,.T.);
#16015=ORIENTED_EDGE('',*,*,#11068,.T.);
#16016=ORIENTED_EDGE('',*,*,#11067,.F.);
#16017=ORIENTED_EDGE('',*,*,#11069,.F.);
#16018=ORIENTED_EDGE('',*,*,#11070,.T.);
#16019=ORIENTED_EDGE('',*,*,#11071,.T.);
#16020=ORIENTED_EDGE('',*,*,#11070,.F.);
#16021=ORIENTED_EDGE('',*,*,#11072,.F.);
#16022=ORIENTED_EDGE('',*,*,#11073,.T.);
#16023=ORIENTED_EDGE('',*,*,#11074,.T.);
#16024=ORIENTED_EDGE('',*,*,#11073,.F.);
#16025=ORIENTED_EDGE('',*,*,#11075,.F.);
#16026=ORIENTED_EDGE('',*,*,#11076,.T.);
#16027=ORIENTED_EDGE('',*,*,#11077,.T.);
#16028=ORIENTED_EDGE('',*,*,#11076,.F.);
#16029=ORIENTED_EDGE('',*,*,#11078,.F.);
#16030=ORIENTED_EDGE('',*,*,#11079,.T.);
#16031=ORIENTED_EDGE('',*,*,#11080,.T.);
#16032=ORIENTED_EDGE('',*,*,#11079,.F.);
#16033=ORIENTED_EDGE('',*,*,#11081,.F.);
#16034=ORIENTED_EDGE('',*,*,#11082,.T.);
#16035=ORIENTED_EDGE('',*,*,#11083,.T.);
#16036=ORIENTED_EDGE('',*,*,#11082,.F.);
#16037=ORIENTED_EDGE('',*,*,#11084,.F.);
#16038=ORIENTED_EDGE('',*,*,#11085,.T.);
#16039=ORIENTED_EDGE('',*,*,#11086,.T.);
#16040=ORIENTED_EDGE('',*,*,#11085,.F.);
#16041=ORIENTED_EDGE('',*,*,#11087,.F.);
#16042=ORIENTED_EDGE('',*,*,#11088,.T.);
#16043=ORIENTED_EDGE('',*,*,#11089,.T.);
#16044=ORIENTED_EDGE('',*,*,#11088,.F.);
#16045=ORIENTED_EDGE('',*,*,#11090,.F.);
#16046=ORIENTED_EDGE('',*,*,#11091,.T.);
#16047=ORIENTED_EDGE('',*,*,#11092,.T.);
#16048=ORIENTED_EDGE('',*,*,#11091,.F.);
#16049=ORIENTED_EDGE('',*,*,#11093,.F.);
#16050=ORIENTED_EDGE('',*,*,#11094,.T.);
#16051=ORIENTED_EDGE('',*,*,#11095,.T.);
#16052=ORIENTED_EDGE('',*,*,#11094,.F.);
#16053=ORIENTED_EDGE('',*,*,#11096,.F.);
#16054=ORIENTED_EDGE('',*,*,#11097,.T.);
#16055=ORIENTED_EDGE('',*,*,#11098,.T.);
#16056=ORIENTED_EDGE('',*,*,#11097,.F.);
#16057=ORIENTED_EDGE('',*,*,#11099,.F.);
#16058=ORIENTED_EDGE('',*,*,#11100,.T.);
#16059=ORIENTED_EDGE('',*,*,#11101,.T.);
#16060=ORIENTED_EDGE('',*,*,#11100,.F.);
#16061=ORIENTED_EDGE('',*,*,#11102,.F.);
#16062=ORIENTED_EDGE('',*,*,#11103,.T.);
#16063=ORIENTED_EDGE('',*,*,#11104,.T.);
#16064=ORIENTED_EDGE('',*,*,#11103,.F.);
#16065=ORIENTED_EDGE('',*,*,#11105,.F.);
#16066=ORIENTED_EDGE('',*,*,#11106,.T.);
#16067=ORIENTED_EDGE('',*,*,#11107,.T.);
#16068=ORIENTED_EDGE('',*,*,#11106,.F.);
#16069=ORIENTED_EDGE('',*,*,#11108,.F.);
#16070=ORIENTED_EDGE('',*,*,#11109,.T.);
#16071=ORIENTED_EDGE('',*,*,#11110,.T.);
#16072=ORIENTED_EDGE('',*,*,#11109,.F.);
#16073=ORIENTED_EDGE('',*,*,#11111,.F.);
#16074=ORIENTED_EDGE('',*,*,#11112,.T.);
#16075=ORIENTED_EDGE('',*,*,#11113,.T.);
#16076=ORIENTED_EDGE('',*,*,#11112,.F.);
#16077=ORIENTED_EDGE('',*,*,#11114,.F.);
#16078=ORIENTED_EDGE('',*,*,#11115,.T.);
#16079=ORIENTED_EDGE('',*,*,#11116,.T.);
#16080=ORIENTED_EDGE('',*,*,#11115,.F.);
#16081=ORIENTED_EDGE('',*,*,#11117,.F.);
#16082=ORIENTED_EDGE('',*,*,#11118,.T.);
#16083=ORIENTED_EDGE('',*,*,#11119,.T.);
#16084=ORIENTED_EDGE('',*,*,#11118,.F.);
#16085=ORIENTED_EDGE('',*,*,#11120,.F.);
#16086=ORIENTED_EDGE('',*,*,#11121,.T.);
#16087=ORIENTED_EDGE('',*,*,#11122,.T.);
#16088=ORIENTED_EDGE('',*,*,#11121,.F.);
#16089=ORIENTED_EDGE('',*,*,#11123,.F.);
#16090=ORIENTED_EDGE('',*,*,#11124,.T.);
#16091=ORIENTED_EDGE('',*,*,#11125,.T.);
#16092=ORIENTED_EDGE('',*,*,#11124,.F.);
#16093=ORIENTED_EDGE('',*,*,#11126,.F.);
#16094=ORIENTED_EDGE('',*,*,#11127,.T.);
#16095=ORIENTED_EDGE('',*,*,#11128,.T.);
#16096=ORIENTED_EDGE('',*,*,#11127,.F.);
#16097=ORIENTED_EDGE('',*,*,#11129,.F.);
#16098=ORIENTED_EDGE('',*,*,#11130,.T.);
#16099=ORIENTED_EDGE('',*,*,#11131,.T.);
#16100=ORIENTED_EDGE('',*,*,#11130,.F.);
#16101=ORIENTED_EDGE('',*,*,#11132,.F.);
#16102=ORIENTED_EDGE('',*,*,#11133,.T.);
#16103=ORIENTED_EDGE('',*,*,#11134,.T.);
#16104=ORIENTED_EDGE('',*,*,#11133,.F.);
#16105=ORIENTED_EDGE('',*,*,#11135,.F.);
#16106=ORIENTED_EDGE('',*,*,#11136,.T.);
#16107=ORIENTED_EDGE('',*,*,#11137,.T.);
#16108=ORIENTED_EDGE('',*,*,#11136,.F.);
#16109=ORIENTED_EDGE('',*,*,#11138,.F.);
#16110=ORIENTED_EDGE('',*,*,#11139,.T.);
#16111=ORIENTED_EDGE('',*,*,#11140,.T.);
#16112=ORIENTED_EDGE('',*,*,#11139,.F.);
#16113=ORIENTED_EDGE('',*,*,#11141,.F.);
#16114=ORIENTED_EDGE('',*,*,#11142,.T.);
#16115=ORIENTED_EDGE('',*,*,#11143,.T.);
#16116=ORIENTED_EDGE('',*,*,#11142,.F.);
#16117=ORIENTED_EDGE('',*,*,#11144,.F.);
#16118=ORIENTED_EDGE('',*,*,#11145,.T.);
#16119=ORIENTED_EDGE('',*,*,#11146,.T.);
#16120=ORIENTED_EDGE('',*,*,#11145,.F.);
#16121=ORIENTED_EDGE('',*,*,#11147,.F.);
#16122=ORIENTED_EDGE('',*,*,#11148,.T.);
#16123=ORIENTED_EDGE('',*,*,#11149,.T.);
#16124=ORIENTED_EDGE('',*,*,#11148,.F.);
#16125=ORIENTED_EDGE('',*,*,#11150,.F.);
#16126=ORIENTED_EDGE('',*,*,#11151,.T.);
#16127=ORIENTED_EDGE('',*,*,#11152,.T.);
#16128=ORIENTED_EDGE('',*,*,#11151,.F.);
#16129=ORIENTED_EDGE('',*,*,#11153,.F.);
#16130=ORIENTED_EDGE('',*,*,#11154,.T.);
#16131=ORIENTED_EDGE('',*,*,#11155,.T.);
#16132=ORIENTED_EDGE('',*,*,#11154,.F.);
#16133=ORIENTED_EDGE('',*,*,#11156,.F.);
#16134=ORIENTED_EDGE('',*,*,#11157,.T.);
#16135=ORIENTED_EDGE('',*,*,#11158,.T.);
#16136=ORIENTED_EDGE('',*,*,#11157,.F.);
#16137=ORIENTED_EDGE('',*,*,#11159,.F.);
#16138=ORIENTED_EDGE('',*,*,#11160,.T.);
#16139=ORIENTED_EDGE('',*,*,#11161,.T.);
#16140=ORIENTED_EDGE('',*,*,#11160,.F.);
#16141=ORIENTED_EDGE('',*,*,#11162,.F.);
#16142=ORIENTED_EDGE('',*,*,#11163,.T.);
#16143=ORIENTED_EDGE('',*,*,#11164,.T.);
#16144=ORIENTED_EDGE('',*,*,#11163,.F.);
#16145=ORIENTED_EDGE('',*,*,#11165,.F.);
#16146=ORIENTED_EDGE('',*,*,#11166,.T.);
#16147=ORIENTED_EDGE('',*,*,#11167,.T.);
#16148=ORIENTED_EDGE('',*,*,#11166,.F.);
#16149=ORIENTED_EDGE('',*,*,#11168,.F.);
#16150=ORIENTED_EDGE('',*,*,#11169,.T.);
#16151=ORIENTED_EDGE('',*,*,#11170,.T.);
#16152=ORIENTED_EDGE('',*,*,#11169,.F.);
#16153=ORIENTED_EDGE('',*,*,#11171,.F.);
#16154=ORIENTED_EDGE('',*,*,#11172,.T.);
#16155=ORIENTED_EDGE('',*,*,#11173,.T.);
#16156=ORIENTED_EDGE('',*,*,#11172,.F.);
#16157=ORIENTED_EDGE('',*,*,#11174,.F.);
#16158=ORIENTED_EDGE('',*,*,#11175,.T.);
#16159=ORIENTED_EDGE('',*,*,#11176,.T.);
#16160=ORIENTED_EDGE('',*,*,#11175,.F.);
#16161=ORIENTED_EDGE('',*,*,#11177,.F.);
#16162=ORIENTED_EDGE('',*,*,#11050,.T.);
#16163=ORIENTED_EDGE('',*,*,#11176,.F.);
#16164=ORIENTED_EDGE('',*,*,#11049,.F.);
#16165=ORIENTED_EDGE('',*,*,#11055,.F.);
#16166=ORIENTED_EDGE('',*,*,#11056,.F.);
#16167=ORIENTED_EDGE('',*,*,#11059,.F.);
#16168=ORIENTED_EDGE('',*,*,#11062,.F.);
#16169=ORIENTED_EDGE('',*,*,#11065,.F.);
#16170=ORIENTED_EDGE('',*,*,#11068,.F.);
#16171=ORIENTED_EDGE('',*,*,#11071,.F.);
#16172=ORIENTED_EDGE('',*,*,#11074,.F.);
#16173=ORIENTED_EDGE('',*,*,#11077,.F.);
#16174=ORIENTED_EDGE('',*,*,#11080,.F.);
#16175=ORIENTED_EDGE('',*,*,#11083,.F.);
#16176=ORIENTED_EDGE('',*,*,#11086,.F.);
#16177=ORIENTED_EDGE('',*,*,#11089,.F.);
#16178=ORIENTED_EDGE('',*,*,#11092,.F.);
#16179=ORIENTED_EDGE('',*,*,#11095,.F.);
#16180=ORIENTED_EDGE('',*,*,#11098,.F.);
#16181=ORIENTED_EDGE('',*,*,#11101,.F.);
#16182=ORIENTED_EDGE('',*,*,#11104,.F.);
#16183=ORIENTED_EDGE('',*,*,#11107,.F.);
#16184=ORIENTED_EDGE('',*,*,#11110,.F.);
#16185=ORIENTED_EDGE('',*,*,#11113,.F.);
#16186=ORIENTED_EDGE('',*,*,#11116,.F.);
#16187=ORIENTED_EDGE('',*,*,#11119,.F.);
#16188=ORIENTED_EDGE('',*,*,#11122,.F.);
#16189=ORIENTED_EDGE('',*,*,#11125,.F.);
#16190=ORIENTED_EDGE('',*,*,#11128,.F.);
#16191=ORIENTED_EDGE('',*,*,#11131,.F.);
#16192=ORIENTED_EDGE('',*,*,#11134,.F.);
#16193=ORIENTED_EDGE('',*,*,#11137,.F.);
#16194=ORIENTED_EDGE('',*,*,#11140,.F.);
#16195=ORIENTED_EDGE('',*,*,#11143,.F.);
#16196=ORIENTED_EDGE('',*,*,#11146,.F.);
#16197=ORIENTED_EDGE('',*,*,#11149,.F.);
#16198=ORIENTED_EDGE('',*,*,#11152,.F.);
#16199=ORIENTED_EDGE('',*,*,#11155,.F.);
#16200=ORIENTED_EDGE('',*,*,#11158,.F.);
#16201=ORIENTED_EDGE('',*,*,#11161,.F.);
#16202=ORIENTED_EDGE('',*,*,#11164,.F.);
#16203=ORIENTED_EDGE('',*,*,#11167,.F.);
#16204=ORIENTED_EDGE('',*,*,#11170,.F.);
#16205=ORIENTED_EDGE('',*,*,#11173,.F.);
#16206=ORIENTED_EDGE('',*,*,#11048,.T.);
#16207=ORIENTED_EDGE('',*,*,#11177,.T.);
#16208=ORIENTED_EDGE('',*,*,#11174,.T.);
#16209=ORIENTED_EDGE('',*,*,#11171,.T.);
#16210=ORIENTED_EDGE('',*,*,#11168,.T.);
#16211=ORIENTED_EDGE('',*,*,#11165,.T.);
#16212=ORIENTED_EDGE('',*,*,#11162,.T.);
#16213=ORIENTED_EDGE('',*,*,#11159,.T.);
#16214=ORIENTED_EDGE('',*,*,#11156,.T.);
#16215=ORIENTED_EDGE('',*,*,#11153,.T.);
#16216=ORIENTED_EDGE('',*,*,#11150,.T.);
#16217=ORIENTED_EDGE('',*,*,#11147,.T.);
#16218=ORIENTED_EDGE('',*,*,#11144,.T.);
#16219=ORIENTED_EDGE('',*,*,#11141,.T.);
#16220=ORIENTED_EDGE('',*,*,#11138,.T.);
#16221=ORIENTED_EDGE('',*,*,#11135,.T.);
#16222=ORIENTED_EDGE('',*,*,#11132,.T.);
#16223=ORIENTED_EDGE('',*,*,#11129,.T.);
#16224=ORIENTED_EDGE('',*,*,#11126,.T.);
#16225=ORIENTED_EDGE('',*,*,#11123,.T.);
#16226=ORIENTED_EDGE('',*,*,#11120,.T.);
#16227=ORIENTED_EDGE('',*,*,#11117,.T.);
#16228=ORIENTED_EDGE('',*,*,#11114,.T.);
#16229=ORIENTED_EDGE('',*,*,#11111,.T.);
#16230=ORIENTED_EDGE('',*,*,#11108,.T.);
#16231=ORIENTED_EDGE('',*,*,#11105,.T.);
#16232=ORIENTED_EDGE('',*,*,#11102,.T.);
#16233=ORIENTED_EDGE('',*,*,#11099,.T.);
#16234=ORIENTED_EDGE('',*,*,#11096,.T.);
#16235=ORIENTED_EDGE('',*,*,#11093,.T.);
#16236=ORIENTED_EDGE('',*,*,#11090,.T.);
#16237=ORIENTED_EDGE('',*,*,#11087,.T.);
#16238=ORIENTED_EDGE('',*,*,#11084,.T.);
#16239=ORIENTED_EDGE('',*,*,#11081,.T.);
#16240=ORIENTED_EDGE('',*,*,#11078,.T.);
#16241=ORIENTED_EDGE('',*,*,#11075,.T.);
#16242=ORIENTED_EDGE('',*,*,#11072,.T.);
#16243=ORIENTED_EDGE('',*,*,#11069,.T.);
#16244=ORIENTED_EDGE('',*,*,#11066,.T.);
#16245=ORIENTED_EDGE('',*,*,#11063,.T.);
#16246=ORIENTED_EDGE('',*,*,#11060,.T.);
#16247=ORIENTED_EDGE('',*,*,#11057,.T.);
#16248=ORIENTED_EDGE('',*,*,#11053,.T.);
#16249=ORIENTED_EDGE('',*,*,#11051,.T.);
#16250=ORIENTED_EDGE('',*,*,#10863,.F.);
#16251=ORIENTED_EDGE('',*,*,#10861,.T.);
#16252=ORIENTED_EDGE('',*,*,#11178,.T.);
#16253=ORIENTED_EDGE('',*,*,#11179,.T.);
#16254=ORIENTED_EDGE('',*,*,#11180,.T.);
#16255=ORIENTED_EDGE('',*,*,#11179,.F.);
#16256=ORIENTED_EDGE('',*,*,#11181,.T.);
#16257=ORIENTED_EDGE('',*,*,#11182,.F.);
#16258=ORIENTED_EDGE('',*,*,#11183,.F.);
#16259=ORIENTED_EDGE('',*,*,#11184,.T.);
#16260=ORIENTED_EDGE('',*,*,#11185,.F.);
#16261=ORIENTED_EDGE('',*,*,#11186,.T.);
#16262=ORIENTED_EDGE('',*,*,#11187,.T.);
#16263=ORIENTED_EDGE('',*,*,#11184,.F.);
#16264=ORIENTED_EDGE('',*,*,#11188,.T.);
#16265=ORIENTED_EDGE('',*,*,#11186,.F.);
#16266=ORIENTED_EDGE('',*,*,#11189,.F.);
#16267=ORIENTED_EDGE('',*,*,#11190,.T.);
#16268=ORIENTED_EDGE('',*,*,#11191,.T.);
#16269=ORIENTED_EDGE('',*,*,#11190,.F.);
#16270=ORIENTED_EDGE('',*,*,#11192,.F.);
#16271=ORIENTED_EDGE('',*,*,#11193,.T.);
#16272=ORIENTED_EDGE('',*,*,#11194,.T.);
#16273=ORIENTED_EDGE('',*,*,#11193,.F.);
#16274=ORIENTED_EDGE('',*,*,#11195,.F.);
#16275=ORIENTED_EDGE('',*,*,#11196,.T.);
#16276=ORIENTED_EDGE('',*,*,#11197,.T.);
#16277=ORIENTED_EDGE('',*,*,#11196,.F.);
#16278=ORIENTED_EDGE('',*,*,#11198,.F.);
#16279=ORIENTED_EDGE('',*,*,#11199,.T.);
#16280=ORIENTED_EDGE('',*,*,#11200,.T.);
#16281=ORIENTED_EDGE('',*,*,#11199,.F.);
#16282=ORIENTED_EDGE('',*,*,#11201,.F.);
#16283=ORIENTED_EDGE('',*,*,#11202,.T.);
#16284=ORIENTED_EDGE('',*,*,#11203,.T.);
#16285=ORIENTED_EDGE('',*,*,#11202,.F.);
#16286=ORIENTED_EDGE('',*,*,#11204,.F.);
#16287=ORIENTED_EDGE('',*,*,#11205,.T.);
#16288=ORIENTED_EDGE('',*,*,#11206,.T.);
#16289=ORIENTED_EDGE('',*,*,#11205,.F.);
#16290=ORIENTED_EDGE('',*,*,#11207,.F.);
#16291=ORIENTED_EDGE('',*,*,#11208,.T.);
#16292=ORIENTED_EDGE('',*,*,#11209,.T.);
#16293=ORIENTED_EDGE('',*,*,#11208,.F.);
#16294=ORIENTED_EDGE('',*,*,#11210,.F.);
#16295=ORIENTED_EDGE('',*,*,#11211,.T.);
#16296=ORIENTED_EDGE('',*,*,#11212,.T.);
#16297=ORIENTED_EDGE('',*,*,#11211,.F.);
#16298=ORIENTED_EDGE('',*,*,#11213,.F.);
#16299=ORIENTED_EDGE('',*,*,#11182,.T.);
#16300=ORIENTED_EDGE('',*,*,#11212,.F.);
#16301=ORIENTED_EDGE('',*,*,#11181,.F.);
#16302=ORIENTED_EDGE('',*,*,#11187,.F.);
#16303=ORIENTED_EDGE('',*,*,#11188,.F.);
#16304=ORIENTED_EDGE('',*,*,#11191,.F.);
#16305=ORIENTED_EDGE('',*,*,#11194,.F.);
#16306=ORIENTED_EDGE('',*,*,#11197,.F.);
#16307=ORIENTED_EDGE('',*,*,#11200,.F.);
#16308=ORIENTED_EDGE('',*,*,#11203,.F.);
#16309=ORIENTED_EDGE('',*,*,#11206,.F.);
#16310=ORIENTED_EDGE('',*,*,#11209,.F.);
#16311=ORIENTED_EDGE('',*,*,#11178,.F.);
#16312=ORIENTED_EDGE('',*,*,#11213,.T.);
#16313=ORIENTED_EDGE('',*,*,#11210,.T.);
#16314=ORIENTED_EDGE('',*,*,#11207,.T.);
#16315=ORIENTED_EDGE('',*,*,#11204,.T.);
#16316=ORIENTED_EDGE('',*,*,#11201,.T.);
#16317=ORIENTED_EDGE('',*,*,#11198,.T.);
#16318=ORIENTED_EDGE('',*,*,#11195,.T.);
#16319=ORIENTED_EDGE('',*,*,#11192,.T.);
#16320=ORIENTED_EDGE('',*,*,#11189,.T.);
#16321=ORIENTED_EDGE('',*,*,#11185,.T.);
#16322=ORIENTED_EDGE('',*,*,#11183,.T.);
#16323=ORIENTED_EDGE('',*,*,#11180,.F.);
#16324=PLANE('',#17917);
#16325=PLANE('',#17944);
#16326=PLANE('',#17971);
#16327=PLANE('',#17998);
#16328=PLANE('',#17999);
#16329=PLANE('',#18000);
#16330=PLANE('',#18001);
#16331=PLANE('',#18002);
#16332=PLANE('',#18003);
#16333=PLANE('',#18004);
#16334=PLANE('',#18005);
#16335=PLANE('',#18006);
#16336=PLANE('',#18007);
#16337=PLANE('',#18008);
#16338=PLANE('',#18009);
#16339=PLANE('',#18010);
#16340=PLANE('',#18011);
#16341=PLANE('',#18012);
#16342=PLANE('',#18013);
#16343=PLANE('',#18014);
#16344=PLANE('',#18015);
#16345=PLANE('',#18016);
#16346=PLANE('',#18017);
#16347=PLANE('',#18018);
#16348=PLANE('',#18019);
#16349=PLANE('',#18020);
#16350=PLANE('',#18021);
#16351=PLANE('',#18022);
#16352=PLANE('',#18023);
#16353=PLANE('',#18024);
#16354=PLANE('',#18025);
#16355=PLANE('',#18026);
#16356=PLANE('',#18027);
#16357=PLANE('',#18028);
#16358=PLANE('',#18029);
#16359=PLANE('',#18030);
#16360=PLANE('',#18031);
#16361=PLANE('',#18032);
#16362=PLANE('',#18033);
#16363=PLANE('',#18034);
#16364=PLANE('',#18035);
#16365=PLANE('',#18036);
#16366=PLANE('',#18037);
#16367=PLANE('',#18038);
#16368=PLANE('',#18039);
#16369=PLANE('',#18040);
#16370=PLANE('',#18041);
#16371=PLANE('',#18042);
#16372=PLANE('',#18043);
#16373=PLANE('',#18044);
#16374=PLANE('',#18045);
#16375=PLANE('',#18046);
#16376=PLANE('',#18047);
#16377=PLANE('',#18048);
#16378=PLANE('',#18049);
#16379=PLANE('',#18050);
#16380=PLANE('',#18051);
#16381=PLANE('',#18052);
#16382=PLANE('',#18053);
#16383=PLANE('',#18054);
#16384=PLANE('',#18055);
#16385=PLANE('',#18056);
#16386=PLANE('',#18057);
#16387=PLANE('',#18058);
#16388=PLANE('',#18059);
#16389=PLANE('',#18060);
#16390=PLANE('',#18061);
#16391=PLANE('',#18062);
#16392=PLANE('',#18063);
#16393=PLANE('',#18064);
#16394=PLANE('',#18065);
#16395=PLANE('',#18066);
#16396=PLANE('',#18067);
#16397=PLANE('',#18068);
#16398=PLANE('',#18069);
#16399=PLANE('',#18070);
#16400=PLANE('',#18071);
#16401=PLANE('',#18072);
#16402=PLANE('',#18073);
#16403=PLANE('',#18074);
#16404=PLANE('',#18075);
#16405=PLANE('',#18076);
#16406=PLANE('',#18077);
#16407=PLANE('',#18078);
#16408=PLANE('',#18079);
#16409=PLANE('',#18080);
#16410=PLANE('',#18081);
#16411=PLANE('',#18082);
#16412=PLANE('',#18083);
#16413=PLANE('',#18084);
#16414=PLANE('',#18085);
#16415=PLANE('',#18086);
#16416=PLANE('',#18087);
#16417=PLANE('',#18088);
#16418=PLANE('',#18089);
#16419=PLANE('',#18090);
#16420=PLANE('',#18091);
#16421=PLANE('',#18092);
#16422=PLANE('',#18093);
#16423=PLANE('',#18094);
#16424=PLANE('',#18095);
#16425=PLANE('',#18096);
#16426=PLANE('',#18097);
#16427=PLANE('',#18098);
#16428=PLANE('',#18099);
#16429=PLANE('',#18100);
#16430=PLANE('',#18101);
#16431=PLANE('',#18102);
#16432=PLANE('',#18103);
#16433=PLANE('',#18104);
#16434=PLANE('',#18149);
#16435=PLANE('',#18151);
#16436=PLANE('',#18152);
#16437=PLANE('',#18153);
#16438=PLANE('',#18154);
#16439=PLANE('',#18156);
#16440=PLANE('',#18163);
#16441=PLANE('',#18164);
#16442=PLANE('',#18165);
#16443=PLANE('',#18166);
#16444=PLANE('',#18179);
#16445=PLANE('',#18180);
#16446=PLANE('',#18181);
#16447=PLANE('',#18182);
#16448=PLANE('',#18183);
#16449=PLANE('',#18184);
#16450=PLANE('',#18185);
#16451=PLANE('',#18186);
#16452=PLANE('',#18187);
#16453=PLANE('',#18188);
#16454=PLANE('',#18189);
#16455=PLANE('',#18190);
#16456=PLANE('',#18191);
#16457=PLANE('',#18192);
#16458=PLANE('',#18193);
#16459=PLANE('',#18194);
#16460=PLANE('',#18195);
#16461=PLANE('',#18196);
#16462=PLANE('',#18210);
#16463=PLANE('',#18211);
#16464=PLANE('',#18212);
#16465=PLANE('',#18213);
#16466=PLANE('',#18214);
#16467=PLANE('',#18215);
#16468=PLANE('',#18216);
#16469=PLANE('',#18217);
#16470=PLANE('',#18218);
#16471=PLANE('',#18221);
#16472=PLANE('',#18224);
#16473=PLANE('',#18225);
#16474=PLANE('',#18228);
#16475=PLANE('',#18234);
#16476=PLANE('',#18238);
#16477=PLANE('',#18242);
#16478=PLANE('',#18246);
#16479=PLANE('',#18247);
#16480=PLANE('',#18249);
#16481=PLANE('',#18250);
#16482=PLANE('',#18252);
#16483=PLANE('',#18255);
#16484=PLANE('',#18256);
#16485=PLANE('',#18257);
#16486=PLANE('',#18259);
#16487=PLANE('',#18260);
#16488=PLANE('',#18264);
#16489=PLANE('',#18265);
#16490=PLANE('',#18266);
#16491=PLANE('',#18267);
#16492=PLANE('',#18268);
#16493=PLANE('',#18269);
#16494=PLANE('',#18371);
#16495=PLANE('',#18373);
#16496=PLANE('',#18375);
#16497=PLANE('',#18379);
#16498=PLANE('',#18534);
#16499=PLANE('',#18535);
#16500=PLANE('',#18536);
#16501=PLANE('',#18537);
#16502=PLANE('',#18538);
#16503=PLANE('',#18539);
#16504=PLANE('',#18540);
#16505=PLANE('',#18541);
#16506=PLANE('',#18542);
#16507=PLANE('',#18543);
#16508=PLANE('',#18544);
#16509=PLANE('',#18545);
#16510=PLANE('',#18546);
#16511=PLANE('',#18547);
#16512=PLANE('',#18548);
#16513=PLANE('',#18549);
#16514=PLANE('',#18556);
#16515=PLANE('',#18558);
#16516=PLANE('',#18560);
#16517=PLANE('',#18561);
#16518=PLANE('',#18562);
#16519=PLANE('',#18563);
#16520=PLANE('',#18635);
#16521=PLANE('',#18636);
#16522=PLANE('',#18640);
#16523=PLANE('',#18641);
#16524=PLANE('',#18642);
#16525=PLANE('',#18643);
#16526=PLANE('',#18653);
#16527=PLANE('',#18654);
#16528=PLANE('',#18655);
#16529=PLANE('',#18656);
#16530=PLANE('',#18657);
#16531=PLANE('',#18658);
#16532=PLANE('',#18659);
#16533=PLANE('',#18660);
#16534=PLANE('',#18696);
#16535=PLANE('',#18697);
#16536=PLANE('',#18698);
#16537=PLANE('',#18699);
#16538=PLANE('',#18703);
#16539=PLANE('',#18704);
#16540=PLANE('',#18708);
#16541=PLANE('',#18712);
#16542=PLANE('',#18713);
#16543=PLANE('',#18714);
#16544=PLANE('',#18715);
#16545=PLANE('',#18716);
#16546=PLANE('',#18717);
#16547=PLANE('',#18718);
#16548=PLANE('',#18719);
#16549=PLANE('',#18720);
#16550=PLANE('',#18721);
#16551=PLANE('',#18722);
#16552=PLANE('',#18723);
#16553=PLANE('',#18724);
#16554=PLANE('',#18725);
#16555=PLANE('',#18733);
#16556=PLANE('',#18742);
#16557=PLANE('',#18745);
#16558=PLANE('',#18748);
#16559=PLANE('',#18749);
#16560=PLANE('',#18750);
#16561=PLANE('',#18751);
#16562=PLANE('',#18752);
#16563=PLANE('',#18753);
#16564=PLANE('',#18754);
#16565=PLANE('',#18756);
#16566=PLANE('',#18757);
#16567=PLANE('',#18770);
#16568=PLANE('',#18771);
#16569=PLANE('',#18772);
#16570=PLANE('',#18773);
#16571=PLANE('',#18774);
#16572=PLANE('',#18775);
#16573=PLANE('',#18776);
#16574=PLANE('',#18777);
#16575=PLANE('',#18778);
#16576=PLANE('',#18779);
#16577=PLANE('',#18780);
#16578=PLANE('',#18781);
#16579=PLANE('',#18782);
#16580=PLANE('',#18783);
#16581=PLANE('',#18784);
#16582=PLANE('',#18785);
#16583=PLANE('',#18786);
#16584=PLANE('',#18850);
#16585=PLANE('',#18852);
#16586=PLANE('',#18853);
#16587=PLANE('',#18854);
#16588=PLANE('',#18855);
#16589=PLANE('',#18857);
#16590=PLANE('',#18858);
#16591=PLANE('',#18859);
#16592=PLANE('',#18860);
#16593=PLANE('',#18862);
#16594=PLANE('',#18863);
#16595=PLANE('',#18864);
#16596=PLANE('',#18865);
#16597=PLANE('',#18868);
#16598=PLANE('',#18869);
#16599=PLANE('',#18870);
#16600=PLANE('',#18874);
#16601=PLANE('',#18881);
#16602=PLANE('',#18898);
#16603=PLANE('',#18899);
#16604=PLANE('',#18900);
#16605=PLANE('',#18901);
#16606=PLANE('',#18902);
#16607=PLANE('',#18910);
#16608=PLANE('',#18924);
#16609=PLANE('',#18925);
#16610=PLANE('',#18937);
#16611=PLANE('',#18939);
#16612=PLANE('',#18942);
#16613=PLANE('',#18944);
#16614=PLANE('',#18946);
#16615=PLANE('',#18965);
#16616=PLANE('',#18966);
#16617=PLANE('',#18967);
#16618=PLANE('',#18968);
#16619=PLANE('',#18969);
#16620=PLANE('',#18970);
#16621=PLANE('',#18971);
#16622=PLANE('',#18972);
#16623=PLANE('',#18973);
#16624=PLANE('',#18974);
#16625=PLANE('',#18975);
#16626=PLANE('',#18976);
#16627=PLANE('',#18977);
#16628=PLANE('',#18978);
#16629=PLANE('',#18979);
#16630=PLANE('',#18980);
#16631=PLANE('',#18981);
#16632=PLANE('',#18982);
#16633=PLANE('',#18983);
#16634=PLANE('',#18984);
#16635=PLANE('',#18985);
#16636=PLANE('',#18986);
#16637=PLANE('',#18987);
#16638=PLANE('',#18988);
#16639=PLANE('',#18989);
#16640=PLANE('',#18990);
#16641=PLANE('',#18991);
#16642=PLANE('',#18992);
#16643=PLANE('',#18993);
#16644=PLANE('',#18994);
#16645=PLANE('',#18995);
#16646=PLANE('',#18996);
#16647=PLANE('',#18997);
#16648=PLANE('',#18998);
#16649=PLANE('',#18999);
#16650=PLANE('',#19000);
#16651=PLANE('',#19001);
#16652=PLANE('',#19002);
#16653=PLANE('',#19003);
#16654=PLANE('',#19004);
#16655=PLANE('',#19005);
#16656=PLANE('',#19006);
#16657=PLANE('',#19007);
#16658=PLANE('',#19008);
#16659=PLANE('',#19009);
#16660=PLANE('',#19010);
#16661=PLANE('',#19011);
#16662=PLANE('',#19012);
#16663=PLANE('',#19013);
#16664=PLANE('',#19014);
#16665=PLANE('',#19015);
#16666=PLANE('',#19016);
#16667=PLANE('',#19017);
#16668=PLANE('',#19018);
#16669=PLANE('',#19019);
#16670=PLANE('',#19020);
#16671=PLANE('',#19021);
#16672=PLANE('',#19022);
#16673=PLANE('',#19023);
#16674=PLANE('',#19024);
#16675=PLANE('',#19025);
#16676=PLANE('',#19026);
#16677=PLANE('',#19027);
#16678=PLANE('',#19028);
#16679=PLANE('',#19029);
#16680=PLANE('',#19030);
#16681=PLANE('',#19031);
#16682=PLANE('',#19032);
#16683=PLANE('',#19033);
#16684=PLANE('',#19034);
#16685=PLANE('',#19035);
#16686=PLANE('',#19036);
#16687=PLANE('',#19037);
#16688=PLANE('',#19038);
#16689=PLANE('',#19039);
#16690=PLANE('',#19040);
#16691=PLANE('',#19041);
#16692=PLANE('',#19042);
#16693=PLANE('',#19043);
#16694=PLANE('',#19044);
#16695=PLANE('',#19045);
#16696=PLANE('',#19046);
#16697=PLANE('',#19047);
#16698=PLANE('',#19048);
#16699=PLANE('',#19049);
#16700=PLANE('',#19050);
#16701=PLANE('',#19051);
#16702=PLANE('',#19052);
#16703=PLANE('',#19053);
#16704=PLANE('',#19054);
#16705=PLANE('',#19055);
#16706=PLANE('',#19056);
#16707=PLANE('',#19058);
#16708=PLANE('',#19060);
#16709=PLANE('',#19066);
#16710=PLANE('',#19067);
#16711=PLANE('',#19082);
#16712=PLANE('',#19083);
#16713=PLANE('',#19089);
#16714=PLANE('',#19095);
#16715=PLANE('',#19096);
#16716=PLANE('',#19097);
#16717=PLANE('',#19098);
#16718=PLANE('',#19099);
#16719=PLANE('',#19100);
#16720=PLANE('',#19101);
#16721=PLANE('',#19102);
#16722=PLANE('',#19103);
#16723=PLANE('',#19104);
#16724=PLANE('',#19105);
#16725=PLANE('',#19106);
#16726=PLANE('',#19107);
#16727=PLANE('',#19108);
#16728=PLANE('',#19109);
#16729=PLANE('',#19110);
#16730=PLANE('',#19111);
#16731=PLANE('',#19112);
#16732=PLANE('',#19113);
#16733=PLANE('',#19114);
#16734=PLANE('',#19115);
#16735=PLANE('',#19116);
#16736=PLANE('',#19117);
#16737=PLANE('',#19119);
#16738=PLANE('',#19125);
#16739=PLANE('',#19126);
#16740=PLANE('',#19127);
#16741=PLANE('',#19128);
#16742=PLANE('',#19129);
#16743=PLANE('',#19130);
#16744=PLANE('',#19131);
#16745=PLANE('',#19134);
#16746=PLANE('',#19137);
#16747=PLANE('',#19140);
#16748=PLANE('',#19141);
#16749=PLANE('',#19142);
#16750=PLANE('',#19143);
#16751=PLANE('',#19145);
#16752=PLANE('',#19151);
#16753=PLANE('',#19152);
#16754=PLANE('',#19153);
#16755=PLANE('',#19154);
#16756=PLANE('',#19155);
#16757=PLANE('',#19156);
#16758=PLANE('',#19157);
#16759=PLANE('',#19158);
#16760=PLANE('',#19159);
#16761=PLANE('',#19160);
#16762=PLANE('',#19161);
#16763=PLANE('',#19162);
#16764=PLANE('',#19163);
#16765=PLANE('',#19164);
#16766=PLANE('',#19165);
#16767=PLANE('',#19166);
#16768=PLANE('',#19167);
#16769=PLANE('',#19169);
#16770=PLANE('',#19237);
#16771=PLANE('',#19238);
#16772=PLANE('',#19240);
#16773=PLANE('',#19246);
#16774=PLANE('',#19247);
#16775=PLANE('',#19257);
#16776=PLANE('',#19259);
#16777=PLANE('',#19277);
#16778=PLANE('',#19282);
#16779=PLANE('',#19285);
#16780=PLANE('',#19290);
#16781=PLANE('',#19291);
#16782=PLANE('',#19292);
#16783=PLANE('',#19293);
#16784=PLANE('',#19295);
#16785=PLANE('',#19296);
#16786=PLANE('',#19297);
#16787=PLANE('',#19298);
#16788=PLANE('',#19303);
#16789=PLANE('',#19308);
#16790=PLANE('',#19313);
#16791=PLANE('',#19314);
#16792=PLANE('',#19315);
#16793=PLANE('',#19316);
#16794=PLANE('',#19321);
#16795=PLANE('',#19322);
#16796=PLANE('',#19323);
#16797=PLANE('',#19324);
#16798=PLANE('',#19329);
#16799=PLANE('',#19330);
#16800=PLANE('',#19331);
#16801=PLANE('',#19332);
#16802=PLANE('',#19333);
#16803=PLANE('',#19334);
#16804=PLANE('',#19335);
#16805=PLANE('',#19336);
#16806=PLANE('',#19337);
#16807=PLANE('',#19351);
#16808=PLANE('',#19355);
#16809=PLANE('',#19359);
#16810=PLANE('',#19360);
#16811=PLANE('',#19361);
#16812=PLANE('',#19362);
#16813=PLANE('',#19363);
#16814=PLANE('',#19364);
#16815=PLANE('',#19365);
#16816=PLANE('',#19366);
#16817=PLANE('',#19367);
#16818=PLANE('',#19368);
#16819=PLANE('',#19369);
#16820=PLANE('',#19370);
#16821=PLANE('',#19371);
#16822=PLANE('',#19372);
#16823=PLANE('',#19373);
#16824=PLANE('',#19374);
#16825=PLANE('',#19375);
#16826=PLANE('',#19376);
#16827=PLANE('',#19377);
#16828=PLANE('',#19378);
#16829=PLANE('',#19379);
#16830=PLANE('',#19380);
#16831=PLANE('',#19381);
#16832=PLANE('',#19382);
#16833=PLANE('',#19383);
#16834=PLANE('',#19384);
#16835=PLANE('',#19385);
#16836=PLANE('',#19386);
#16837=PLANE('',#19387);
#16838=PLANE('',#19388);
#16839=PLANE('',#19389);
#16840=PLANE('',#19390);
#16841=PLANE('',#19391);
#16842=PLANE('',#19392);
#16843=PLANE('',#19393);
#16844=PLANE('',#19394);
#16845=PLANE('',#19395);
#16846=PLANE('',#19396);
#16847=PLANE('',#19400);
#16848=PLANE('',#19401);
#16849=PLANE('',#19402);
#16850=PLANE('',#19403);
#16851=PLANE('',#19404);
#16852=PLANE('',#19409);
#16853=PLANE('',#19413);
#16854=PLANE('',#19414);
#16855=PLANE('',#19415);
#16856=PLANE('',#19416);
#16857=PLANE('',#19420);
#16858=PLANE('',#19421);
#16859=PLANE('',#19422);
#16860=PLANE('',#19426);
#16861=PLANE('',#19427);
#16862=ADVANCED_FACE('',(#1527,#776,#777,#778,#779,#780,#781,#782,#783,
#784,#785,#786,#787,#788,#789,#790,#791,#792,#793,#794,#795,#796,#797,#798,
#799,#800,#801,#802,#803,#804,#805,#806,#807,#808,#809,#810,#811,#812,#813,
#814,#815,#816,#817,#818,#819,#820,#821,#822,#823,#824,#825,#826,#827),
#16324,.F.);
#16863=ADVANCED_FACE('',(#1528,#828,#829,#830,#831,#832,#833,#834,#835,
#836,#837,#838,#839,#840,#841,#842,#843,#844,#845,#846,#847,#848,#849,#850,
#851,#852,#853,#854,#855,#856,#857,#858,#859,#860,#861,#862,#863,#864,#865,
#866,#867,#868,#869,#870,#871,#872,#873,#874,#875,#876,#877,#878,#879),
#16325,.T.);
#16864=ADVANCED_FACE('',(#1529),#16326,.T.);
#16865=ADVANCED_FACE('',(#1530),#489,.F.);
#16866=ADVANCED_FACE('',(#1531),#490,.F.);
#16867=ADVANCED_FACE('',(#1532),#491,.F.);
#16868=ADVANCED_FACE('',(#1533),#492,.F.);
#16869=ADVANCED_FACE('',(#1534),#493,.F.);
#16870=ADVANCED_FACE('',(#1535),#494,.F.);
#16871=ADVANCED_FACE('',(#1536),#495,.F.);
#16872=ADVANCED_FACE('',(#1537),#496,.F.);
#16873=ADVANCED_FACE('',(#1538),#497,.F.);
#16874=ADVANCED_FACE('',(#1539),#498,.F.);
#16875=ADVANCED_FACE('',(#1540),#499,.F.);
#16876=ADVANCED_FACE('',(#1541),#500,.F.);
#16877=ADVANCED_FACE('',(#1542),#501,.F.);
#16878=ADVANCED_FACE('',(#1543),#502,.F.);
#16879=ADVANCED_FACE('',(#1544),#503,.F.);
#16880=ADVANCED_FACE('',(#1545),#504,.F.);
#16881=ADVANCED_FACE('',(#1546),#505,.F.);
#16882=ADVANCED_FACE('',(#1547),#506,.F.);
#16883=ADVANCED_FACE('',(#1548),#507,.F.);
#16884=ADVANCED_FACE('',(#1549),#508,.F.);
#16885=ADVANCED_FACE('',(#1550),#509,.F.);
#16886=ADVANCED_FACE('',(#1551),#510,.F.);
#16887=ADVANCED_FACE('',(#1552),#511,.F.);
#16888=ADVANCED_FACE('',(#1553),#512,.F.);
#16889=ADVANCED_FACE('',(#1554),#513,.F.);
#16890=ADVANCED_FACE('',(#1555),#514,.F.);
#16891=ADVANCED_FACE('',(#1556),#16327,.T.);
#16892=ADVANCED_FACE('',(#1557),#16328,.T.);
#16893=ADVANCED_FACE('',(#1558),#16329,.T.);
#16894=ADVANCED_FACE('',(#1559),#16330,.T.);
#16895=ADVANCED_FACE('',(#1560),#16331,.T.);
#16896=ADVANCED_FACE('',(#1561),#16332,.T.);
#16897=ADVANCED_FACE('',(#1562),#16333,.T.);
#16898=ADVANCED_FACE('',(#1563),#16334,.T.);
#16899=ADVANCED_FACE('',(#1564),#16335,.T.);
#16900=ADVANCED_FACE('',(#1565),#16336,.T.);
#16901=ADVANCED_FACE('',(#1566),#16337,.T.);
#16902=ADVANCED_FACE('',(#1567),#16338,.T.);
#16903=ADVANCED_FACE('',(#1568),#16339,.T.);
#16904=ADVANCED_FACE('',(#1569),#16340,.T.);
#16905=ADVANCED_FACE('',(#1570),#16341,.T.);
#16906=ADVANCED_FACE('',(#1571),#16342,.T.);
#16907=ADVANCED_FACE('',(#1572),#16343,.T.);
#16908=ADVANCED_FACE('',(#1573),#16344,.T.);
#16909=ADVANCED_FACE('',(#1574),#16345,.T.);
#16910=ADVANCED_FACE('',(#1575),#16346,.T.);
#16911=ADVANCED_FACE('',(#1576),#16347,.T.);
#16912=ADVANCED_FACE('',(#1577),#16348,.T.);
#16913=ADVANCED_FACE('',(#1578),#16349,.T.);
#16914=ADVANCED_FACE('',(#1579),#16350,.T.);
#16915=ADVANCED_FACE('',(#1580),#16351,.T.);
#16916=ADVANCED_FACE('',(#1581),#16352,.T.);
#16917=ADVANCED_FACE('',(#1582),#16353,.F.);
#16918=ADVANCED_FACE('',(#1583),#16354,.F.);
#16919=ADVANCED_FACE('',(#1584),#16355,.F.);
#16920=ADVANCED_FACE('',(#1585),#16356,.F.);
#16921=ADVANCED_FACE('',(#1586),#16357,.T.);
#16922=ADVANCED_FACE('',(#1587),#16358,.F.);
#16923=ADVANCED_FACE('',(#1588),#16359,.F.);
#16924=ADVANCED_FACE('',(#1589),#16360,.T.);
#16925=ADVANCED_FACE('',(#1590),#16361,.F.);
#16926=ADVANCED_FACE('',(#1591),#16362,.F.);
#16927=ADVANCED_FACE('',(#1592),#16363,.T.);
#16928=ADVANCED_FACE('',(#1593),#16364,.F.);
#16929=ADVANCED_FACE('',(#1594),#16365,.F.);
#16930=ADVANCED_FACE('',(#1595),#16366,.T.);
#16931=ADVANCED_FACE('',(#1596),#16367,.F.);
#16932=ADVANCED_FACE('',(#1597),#16368,.F.);
#16933=ADVANCED_FACE('',(#1598),#16369,.T.);
#16934=ADVANCED_FACE('',(#1599),#16370,.F.);
#16935=ADVANCED_FACE('',(#1600),#16371,.F.);
#16936=ADVANCED_FACE('',(#1601),#16372,.T.);
#16937=ADVANCED_FACE('',(#1602),#16373,.F.);
#16938=ADVANCED_FACE('',(#1603),#16374,.F.);
#16939=ADVANCED_FACE('',(#1604),#16375,.T.);
#16940=ADVANCED_FACE('',(#1605),#16376,.F.);
#16941=ADVANCED_FACE('',(#1606),#16377,.F.);
#16942=ADVANCED_FACE('',(#1607),#16378,.T.);
#16943=ADVANCED_FACE('',(#1608),#16379,.F.);
#16944=ADVANCED_FACE('',(#1609),#16380,.F.);
#16945=ADVANCED_FACE('',(#1610),#16381,.T.);
#16946=ADVANCED_FACE('',(#1611),#16382,.F.);
#16947=ADVANCED_FACE('',(#1612),#16383,.F.);
#16948=ADVANCED_FACE('',(#1613),#16384,.T.);
#16949=ADVANCED_FACE('',(#1614),#16385,.F.);
#16950=ADVANCED_FACE('',(#1615),#16386,.F.);
#16951=ADVANCED_FACE('',(#1616),#16387,.T.);
#16952=ADVANCED_FACE('',(#1617),#16388,.F.);
#16953=ADVANCED_FACE('',(#1618),#16389,.F.);
#16954=ADVANCED_FACE('',(#1619),#16390,.T.);
#16955=ADVANCED_FACE('',(#1620),#16391,.F.);
#16956=ADVANCED_FACE('',(#1621),#16392,.F.);
#16957=ADVANCED_FACE('',(#1622),#16393,.T.);
#16958=ADVANCED_FACE('',(#1623),#16394,.F.);
#16959=ADVANCED_FACE('',(#1624),#16395,.F.);
#16960=ADVANCED_FACE('',(#1625),#16396,.T.);
#16961=ADVANCED_FACE('',(#1626),#16397,.F.);
#16962=ADVANCED_FACE('',(#1627),#16398,.F.);
#16963=ADVANCED_FACE('',(#1628),#16399,.T.);
#16964=ADVANCED_FACE('',(#1629),#16400,.F.);
#16965=ADVANCED_FACE('',(#1630),#16401,.F.);
#16966=ADVANCED_FACE('',(#1631),#16402,.T.);
#16967=ADVANCED_FACE('',(#1632),#16403,.F.);
#16968=ADVANCED_FACE('',(#1633),#16404,.F.);
#16969=ADVANCED_FACE('',(#1634),#16405,.T.);
#16970=ADVANCED_FACE('',(#1635),#16406,.F.);
#16971=ADVANCED_FACE('',(#1636),#16407,.F.);
#16972=ADVANCED_FACE('',(#1637),#16408,.T.);
#16973=ADVANCED_FACE('',(#1638),#16409,.F.);
#16974=ADVANCED_FACE('',(#1639),#16410,.F.);
#16975=ADVANCED_FACE('',(#1640),#16411,.T.);
#16976=ADVANCED_FACE('',(#1641),#16412,.F.);
#16977=ADVANCED_FACE('',(#1642),#16413,.F.);
#16978=ADVANCED_FACE('',(#1643),#16414,.T.);
#16979=ADVANCED_FACE('',(#1644),#16415,.F.);
#16980=ADVANCED_FACE('',(#1645),#16416,.F.);
#16981=ADVANCED_FACE('',(#1646),#16417,.T.);
#16982=ADVANCED_FACE('',(#1647),#16418,.F.);
#16983=ADVANCED_FACE('',(#1648),#16419,.F.);
#16984=ADVANCED_FACE('',(#1649),#16420,.T.);
#16985=ADVANCED_FACE('',(#1650),#16421,.F.);
#16986=ADVANCED_FACE('',(#1651),#16422,.F.);
#16987=ADVANCED_FACE('',(#1652),#16423,.T.);
#16988=ADVANCED_FACE('',(#1653),#16424,.F.);
#16989=ADVANCED_FACE('',(#1654),#16425,.F.);
#16990=ADVANCED_FACE('',(#1655),#16426,.T.);
#16991=ADVANCED_FACE('',(#1656),#16427,.F.);
#16992=ADVANCED_FACE('',(#1657),#16428,.F.);
#16993=ADVANCED_FACE('',(#1658),#16429,.T.);
#16994=ADVANCED_FACE('',(#1659),#16430,.F.);
#16995=ADVANCED_FACE('',(#1660),#16431,.F.);
#16996=ADVANCED_FACE('',(#1661),#16432,.T.);
#16997=ADVANCED_FACE('',(#1662),#16433,.F.);
#16998=ADVANCED_FACE('',(#1663),#515,.T.);
#16999=ADVANCED_FACE('',(#1664),#516,.T.);
#17000=ADVANCED_FACE('',(#1665),#517,.T.);
#17001=ADVANCED_FACE('',(#1666),#518,.T.);
#17002=ADVANCED_FACE('',(#1667),#519,.T.);
#17003=ADVANCED_FACE('',(#1668),#520,.T.);
#17004=ADVANCED_FACE('',(#1669),#521,.T.);
#17005=ADVANCED_FACE('',(#1670),#522,.T.);
#17006=ADVANCED_FACE('',(#1671),#523,.T.);
#17007=ADVANCED_FACE('',(#1672),#407,.F.);
#17008=ADVANCED_FACE('',(#1673),#524,.T.);
#17009=ADVANCED_FACE('',(#1674),#385,.T.);
#17010=ADVANCED_FACE('',(#1675),#525,.T.);
#17011=ADVANCED_FACE('',(#1676),#386,.T.);
#17012=ADVANCED_FACE('',(#1677),#526,.T.);
#17013=ADVANCED_FACE('',(#1678),#408,.F.);
#17014=ADVANCED_FACE('',(#1679),#527,.T.);
#17015=ADVANCED_FACE('',(#1680),#16434,.F.);
#17016=ADVANCED_FACE('',(#1681),#16435,.F.);
#17017=ADVANCED_FACE('',(#1682),#16436,.F.);
#17018=ADVANCED_FACE('',(#1683),#16437,.F.);
#17019=ADVANCED_FACE('',(#1684),#16438,.F.);
#17020=ADVANCED_FACE('',(#1685),#16439,.F.);
#17021=ADVANCED_FACE('',(#1686),#528,.T.);
#17022=ADVANCED_FACE('',(#1687),#529,.F.);
#17023=ADVANCED_FACE('',(#1688),#16440,.T.);
#17024=ADVANCED_FACE('',(#1689,#880),#16441,.T.);
#17025=ADVANCED_FACE('',(#1690),#16442,.T.);
#17026=ADVANCED_FACE('',(#1691),#16443,.T.);
#17027=ADVANCED_FACE('',(#1692),#530,.T.);
#17028=ADVANCED_FACE('',(#1693),#531,.T.);
#17029=ADVANCED_FACE('',(#1694),#532,.F.);
#17030=ADVANCED_FACE('',(#1695),#533,.F.);
#17031=ADVANCED_FACE('',(#1696),#16444,.F.);
#17032=ADVANCED_FACE('',(#1697),#16445,.F.);
#17033=ADVANCED_FACE('',(#1698),#16446,.F.);
#17034=ADVANCED_FACE('',(#1699),#16447,.F.);
#17035=ADVANCED_FACE('',(#1700),#16448,.F.);
#17036=ADVANCED_FACE('',(#1701),#16449,.F.);
#17037=ADVANCED_FACE('',(#1702),#16450,.F.);
#17038=ADVANCED_FACE('',(#1703),#16451,.F.);
#17039=ADVANCED_FACE('',(#1704),#16452,.F.);
#17040=ADVANCED_FACE('',(#1705),#16453,.F.);
#17041=ADVANCED_FACE('',(#1706),#16454,.F.);
#17042=ADVANCED_FACE('',(#1707),#16455,.T.);
#17043=ADVANCED_FACE('',(#1708),#16456,.T.);
#17044=ADVANCED_FACE('',(#1709),#16457,.T.);
#17045=ADVANCED_FACE('',(#1710),#16458,.T.);
#17046=ADVANCED_FACE('',(#1711),#16459,.T.);
#17047=ADVANCED_FACE('',(#1712),#16460,.T.);
#17048=ADVANCED_FACE('',(#1713),#16461,.T.);
#17049=ADVANCED_FACE('',(#1714),#534,.F.);
#17050=ADVANCED_FACE('',(#1715),#535,.F.);
#17051=ADVANCED_FACE('',(#1716),#536,.F.);
#17052=ADVANCED_FACE('',(#1717),#537,.F.);
#17053=ADVANCED_FACE('',(#1718),#538,.T.);
#17054=ADVANCED_FACE('',(#1719),#16462,.F.);
#17055=ADVANCED_FACE('',(#1720),#16463,.F.);
#17056=ADVANCED_FACE('',(#1721),#16464,.F.);
#17057=ADVANCED_FACE('',(#1722),#16465,.F.);
#17058=ADVANCED_FACE('',(#1723),#16466,.T.);
#17059=ADVANCED_FACE('',(#1724),#16467,.F.);
#17060=ADVANCED_FACE('',(#1725),#16468,.F.);
#17061=ADVANCED_FACE('',(#1726),#16469,.F.);
#17062=ADVANCED_FACE('',(#1727),#16470,.F.);
#17063=ADVANCED_FACE('',(#1728),#16471,.F.);
#17064=ADVANCED_FACE('',(#1729),#16472,.F.);
#17065=ADVANCED_FACE('',(#1730),#16473,.F.);
#17066=ADVANCED_FACE('',(#1731),#16474,.F.);
#17067=ADVANCED_FACE('',(#1732),#539,.F.);
#17068=ADVANCED_FACE('',(#1733),#16475,.F.);
#17069=ADVANCED_FACE('',(#1734),#540,.F.);
#17070=ADVANCED_FACE('',(#1735),#16476,.F.);
#17071=ADVANCED_FACE('',(#1736),#541,.F.);
#17072=ADVANCED_FACE('',(#1737),#16477,.F.);
#17073=ADVANCED_FACE('',(#1738),#542,.F.);
#17074=ADVANCED_FACE('',(#1739),#16478,.F.);
#17075=ADVANCED_FACE('',(#1740),#16479,.F.);
#17076=ADVANCED_FACE('',(#1741),#16480,.F.);
#17077=ADVANCED_FACE('',(#1742),#16481,.T.);
#17078=ADVANCED_FACE('',(#1743,#881,#882),#16482,.T.);
#17079=ADVANCED_FACE('',(#1744),#543,.F.);
#17080=ADVANCED_FACE('',(#1745),#16483,.T.);
#17081=ADVANCED_FACE('',(#1746),#16484,.T.);
#17082=ADVANCED_FACE('',(#1747),#16485,.T.);
#17083=ADVANCED_FACE('',(#1748),#544,.T.);
#17084=ADVANCED_FACE('',(#1749,#883,#884),#16486,.T.);
#17085=ADVANCED_FACE('',(#1750),#16487,.T.);
#17086=ADVANCED_FACE('',(#1751),#545,.T.);
#17087=ADVANCED_FACE('',(#1752),#546,.T.);
#17088=ADVANCED_FACE('',(#1753),#16488,.F.);
#17089=ADVANCED_FACE('',(#1754),#16489,.F.);
#17090=ADVANCED_FACE('',(#1755),#16490,.T.);
#17091=ADVANCED_FACE('',(#1756),#16491,.F.);
#17092=ADVANCED_FACE('',(#1757),#16492,.T.);
#17093=ADVANCED_FACE('',(#1758),#16493,.F.);
#17094=ADVANCED_FACE('',(#1759),#387,.T.);
#17095=ADVANCED_FACE('',(#1760),#388,.T.);
#17096=ADVANCED_FACE('',(#1761),#389,.T.);
#17097=ADVANCED_FACE('',(#1762),#390,.T.);
#17098=ADVANCED_FACE('',(#1763),#391,.T.);
#17099=ADVANCED_FACE('',(#1764),#392,.T.);
#17100=ADVANCED_FACE('',(#1765),#393,.T.);
#17101=ADVANCED_FACE('',(#1766),#394,.T.);
#17102=ADVANCED_FACE('',(#1767),#395,.T.);
#17103=ADVANCED_FACE('',(#1768),#396,.T.);
#17104=ADVANCED_FACE('',(#1769),#193,.F.);
#17105=ADVANCED_FACE('',(#1770),#194,.T.);
#17106=ADVANCED_FACE('',(#1771),#195,.F.);
#17107=ADVANCED_FACE('',(#1772),#196,.T.);
#17108=ADVANCED_FACE('',(#1773),#197,.T.);
#17109=ADVANCED_FACE('',(#1774),#198,.T.);
#17110=ADVANCED_FACE('',(#1775),#199,.F.);
#17111=ADVANCED_FACE('',(#1776),#200,.T.);
#17112=ADVANCED_FACE('',(#1777),#201,.T.);
#17113=ADVANCED_FACE('',(#1778),#547,.T.);
#17114=ADVANCED_FACE('',(#1779),#548,.T.);
#17115=ADVANCED_FACE('',(#1780),#168,.T.);
#17116=ADVANCED_FACE('',(#1781,#885),#16494,.F.);
#17117=ADVANCED_FACE('',(#1782),#549,.F.);
#17118=ADVANCED_FACE('',(#1783,#886),#16495,.F.);
#17119=ADVANCED_FACE('',(#1784),#550,.F.);
#17120=ADVANCED_FACE('',(#1785,#887),#16496,.F.);
#17121=ADVANCED_FACE('',(#1786),#551,.T.);
#17122=ADVANCED_FACE('',(#1787),#169,.T.);
#17123=ADVANCED_FACE('',(#1788,#888),#16497,.F.);
#17124=ADVANCED_FACE('',(#1789),#202,.T.);
#17125=ADVANCED_FACE('',(#1790),#203,.F.);
#17126=ADVANCED_FACE('',(#1791),#204,.T.);
#17127=ADVANCED_FACE('',(#1792),#552,.T.);
#17128=ADVANCED_FACE('',(#1793),#397,.T.);
#17129=ADVANCED_FACE('',(#1794),#205,.T.);
#17130=ADVANCED_FACE('',(#1795),#553,.T.);
#17131=ADVANCED_FACE('',(#1796),#554,.T.);
#17132=ADVANCED_FACE('',(#1797),#206,.T.);
#17133=ADVANCED_FACE('',(#1798),#398,.T.);
#17134=ADVANCED_FACE('',(#1799),#207,.T.);
#17135=ADVANCED_FACE('',(#1800),#208,.T.);
#17136=ADVANCED_FACE('',(#1801),#555,.T.);
#17137=ADVANCED_FACE('',(#1802),#556,.T.);
#17138=ADVANCED_FACE('',(#1803),#557,.T.);
#17139=ADVANCED_FACE('',(#1804),#558,.T.);
#17140=ADVANCED_FACE('',(#1805),#559,.T.);
#17141=ADVANCED_FACE('',(#1806),#209,.T.);
#17142=ADVANCED_FACE('',(#1807),#399,.T.);
#17143=ADVANCED_FACE('',(#1808),#210,.T.);
#17144=ADVANCED_FACE('',(#1809),#560,.T.);
#17145=ADVANCED_FACE('',(#1810),#211,.T.);
#17146=ADVANCED_FACE('',(#1811),#561,.T.);
#17147=ADVANCED_FACE('',(#1812),#212,.T.);
#17148=ADVANCED_FACE('',(#1813),#562,.T.);
#17149=ADVANCED_FACE('',(#1814),#400,.T.);
#17150=ADVANCED_FACE('',(#1815),#401,.T.);
#17151=ADVANCED_FACE('',(#1816),#563,.T.);
#17152=ADVANCED_FACE('',(#1817),#213,.T.);
#17153=ADVANCED_FACE('',(#1818),#564,.T.);
#17154=ADVANCED_FACE('',(#1819),#565,.T.);
#17155=ADVANCED_FACE('',(#1820),#566,.T.);
#17156=ADVANCED_FACE('',(#1821),#214,.T.);
#17157=ADVANCED_FACE('',(#1822),#215,.T.);
#17158=ADVANCED_FACE('',(#1823),#216,.T.);
#17159=ADVANCED_FACE('',(#1824),#402,.T.);
#17160=ADVANCED_FACE('',(#1825),#567,.T.);
#17161=ADVANCED_FACE('',(#1826),#568,.T.);
#17162=ADVANCED_FACE('',(#1827),#569,.T.);
#17163=ADVANCED_FACE('',(#1828),#570,.T.);
#17164=ADVANCED_FACE('',(#1829),#571,.T.);
#17165=ADVANCED_FACE('',(#1830),#217,.T.);
#17166=ADVANCED_FACE('',(#1831),#403,.T.);
#17167=ADVANCED_FACE('',(#1832),#218,.T.);
#17168=ADVANCED_FACE('',(#1833),#572,.T.);
#17169=ADVANCED_FACE('',(#1834),#219,.T.);
#17170=ADVANCED_FACE('',(#1835),#573,.T.);
#17171=ADVANCED_FACE('',(#1836),#220,.T.);
#17172=ADVANCED_FACE('',(#1837),#574,.T.);
#17173=ADVANCED_FACE('',(#1838),#404,.T.);
#17174=ADVANCED_FACE('',(#1839),#405,.T.);
#17175=ADVANCED_FACE('',(#1840),#575,.T.);
#17176=ADVANCED_FACE('',(#1841),#221,.T.);
#17177=ADVANCED_FACE('',(#1842),#576,.T.);
#17178=ADVANCED_FACE('',(#1843),#577,.T.);
#17179=ADVANCED_FACE('',(#1844),#578,.T.);
#17180=ADVANCED_FACE('',(#1845),#222,.T.);
#17181=ADVANCED_FACE('',(#1846),#406,.T.);
#17182=ADVANCED_FACE('',(#1847),#223,.T.);
#17183=ADVANCED_FACE('',(#1848),#224,.T.);
#17184=ADVANCED_FACE('',(#1849),#579,.T.);
#17185=ADVANCED_FACE('',(#1850),#580,.T.);
#17186=ADVANCED_FACE('',(#1851),#581,.T.);
#17187=ADVANCED_FACE('',(#1852),#225,.T.);
#17188=ADVANCED_FACE('',(#1853),#16498,.F.);
#17189=ADVANCED_FACE('',(#1854),#16499,.F.);
#17190=ADVANCED_FACE('',(#1855),#16500,.F.);
#17191=ADVANCED_FACE('',(#1856),#16501,.F.);
#17192=ADVANCED_FACE('',(#1857),#16502,.F.);
#17193=ADVANCED_FACE('',(#1858),#16503,.F.);
#17194=ADVANCED_FACE('',(#1859),#16504,.F.);
#17195=ADVANCED_FACE('',(#1860),#16505,.F.);
#17196=ADVANCED_FACE('',(#1861),#16506,.F.);
#17197=ADVANCED_FACE('',(#1862),#16507,.F.);
#17198=ADVANCED_FACE('',(#1863),#16508,.F.);
#17199=ADVANCED_FACE('',(#1864),#16509,.F.);
#17200=ADVANCED_FACE('',(#1865),#16510,.F.);
#17201=ADVANCED_FACE('',(#1866),#16511,.F.);
#17202=ADVANCED_FACE('',(#1867),#16512,.F.);
#17203=ADVANCED_FACE('',(#1868,#889),#16513,.F.);
#17204=ADVANCED_FACE('',(#1869),#226,.T.);
#17205=ADVANCED_FACE('',(#1870),#582,.F.);
#17206=ADVANCED_FACE('',(#1871),#170,.F.);
#17207=ADVANCED_FACE('',(#1872),#16514,.F.);
#17208=ADVANCED_FACE('',(#1873),#583,.T.);
#17209=ADVANCED_FACE('',(#1874,#890),#16515,.F.);
#17210=ADVANCED_FACE('',(#1875),#584,.T.);
#17211=ADVANCED_FACE('',(#1876),#16516,.F.);
#17212=ADVANCED_FACE('',(#1877),#16517,.F.);
#17213=ADVANCED_FACE('',(#1878),#16518,.F.);
#17214=ADVANCED_FACE('',(#1879),#16519,.F.);
#17215=ADVANCED_FACE('',(#1880),#585,.F.);
#17216=ADVANCED_FACE('',(#1881),#586,.F.);
#17217=ADVANCED_FACE('',(#1882),#587,.F.);
#17218=ADVANCED_FACE('',(#1883),#588,.F.);
#17219=ADVANCED_FACE('',(#1884),#589,.F.);
#17220=ADVANCED_FACE('',(#1885),#590,.F.);
#17221=ADVANCED_FACE('',(#1886),#171,.F.);
#17222=ADVANCED_FACE('',(#1887),#172,.F.);
#17223=ADVANCED_FACE('',(#1888),#173,.F.);
#17224=ADVANCED_FACE('',(#1889),#174,.F.);
#17225=ADVANCED_FACE('',(#1890),#175,.F.);
#17226=ADVANCED_FACE('',(#1891),#176,.F.);
#17227=ADVANCED_FACE('',(#1892),#177,.F.);
#17228=ADVANCED_FACE('',(#1893),#178,.F.);
#17229=ADVANCED_FACE('',(#1894),#179,.F.);
#17230=ADVANCED_FACE('',(#1895),#180,.F.);
#17231=ADVANCED_FACE('',(#1896),#181,.F.);
#17232=ADVANCED_FACE('',(#1897),#182,.F.);
#17233=ADVANCED_FACE('',(#1898),#183,.F.);
#17234=ADVANCED_FACE('',(#1899),#16520,.F.);
#17235=ADVANCED_FACE('',(#1900),#16521,.F.);
#17236=ADVANCED_FACE('',(#1901),#16522,.F.);
#17237=ADVANCED_FACE('',(#1902),#16523,.F.);
#17238=ADVANCED_FACE('',(#1903),#16524,.F.);
#17239=ADVANCED_FACE('',(#1904),#16525,.F.);
#17240=ADVANCED_FACE('',(#1905),#591,.F.);
#17241=ADVANCED_FACE('',(#1906),#592,.F.);
#17242=ADVANCED_FACE('',(#1907),#593,.T.);
#17243=ADVANCED_FACE('',(#1908),#594,.T.);
#17244=ADVANCED_FACE('',(#1909),#16526,.T.);
#17245=ADVANCED_FACE('',(#1910),#16527,.T.);
#17246=ADVANCED_FACE('',(#1911),#16528,.T.);
#17247=ADVANCED_FACE('',(#1912),#16529,.T.);
#17248=ADVANCED_FACE('',(#1913),#16530,.T.);
#17249=ADVANCED_FACE('',(#1914),#16531,.T.);
#17250=ADVANCED_FACE('',(#1915),#16532,.T.);
#17251=ADVANCED_FACE('',(#1916),#16533,.T.);
#17252=ADVANCED_FACE('',(#1917),#595,.F.);
#17253=ADVANCED_FACE('',(#1918),#596,.F.);
#17254=ADVANCED_FACE('',(#1919),#597,.F.);
#17255=ADVANCED_FACE('',(#1920),#598,.F.);
#17256=ADVANCED_FACE('',(#1921),#599,.F.);
#17257=ADVANCED_FACE('',(#1922),#600,.F.);
#17258=ADVANCED_FACE('',(#1923),#601,.F.);
#17259=ADVANCED_FACE('',(#1924),#602,.F.);
#17260=ADVANCED_FACE('',(#1925),#603,.F.);
#17261=ADVANCED_FACE('',(#1926),#604,.F.);
#17262=ADVANCED_FACE('',(#1927),#605,.F.);
#17263=ADVANCED_FACE('',(#1928),#606,.F.);
#17264=ADVANCED_FACE('',(#1929),#607,.F.);
#17265=ADVANCED_FACE('',(#1930),#608,.F.);
#17266=ADVANCED_FACE('',(#1931),#609,.F.);
#17267=ADVANCED_FACE('',(#1932),#610,.F.);
#17268=ADVANCED_FACE('',(#1933),#16534,.F.);
#17269=ADVANCED_FACE('',(#1934),#16535,.F.);
#17270=ADVANCED_FACE('',(#1935),#16536,.F.);
#17271=ADVANCED_FACE('',(#1936),#16537,.F.);
#17272=ADVANCED_FACE('',(#1937),#611,.T.);
#17273=ADVANCED_FACE('',(#1938),#16538,.F.);
#17274=ADVANCED_FACE('',(#1939),#16539,.F.);
#17275=ADVANCED_FACE('',(#1940),#612,.T.);
#17276=ADVANCED_FACE('',(#1941),#16540,.F.);
#17277=ADVANCED_FACE('',(#1942),#613,.T.);
#17278=ADVANCED_FACE('',(#1943),#16541,.F.);
#17279=ADVANCED_FACE('',(#1944),#16542,.F.);
#17280=ADVANCED_FACE('',(#1945),#16543,.F.);
#17281=ADVANCED_FACE('',(#1946),#16544,.F.);
#17282=ADVANCED_FACE('',(#1947),#16545,.F.);
#17283=ADVANCED_FACE('',(#1948),#16546,.F.);
#17284=ADVANCED_FACE('',(#1949),#16547,.F.);
#17285=ADVANCED_FACE('',(#1950),#16548,.F.);
#17286=ADVANCED_FACE('',(#1951),#16549,.F.);
#17287=ADVANCED_FACE('',(#1952,#891,#892,#893,#894,#895,#896,#897,#898,
#899,#900,#901,#902,#903,#904,#905,#906,#907),#16550,.F.);
#17288=ADVANCED_FACE('',(#1953,#908,#909,#910,#911,#912,#913,#914,#915,
#916,#917,#918,#919,#920,#921,#922,#923,#924),#16551,.T.);
#17289=ADVANCED_FACE('',(#1954),#16552,.T.);
#17290=ADVANCED_FACE('',(#1955),#16553,.T.);
#17291=ADVANCED_FACE('',(#1956),#16554,.T.);
#17292=ADVANCED_FACE('',(#1957),#614,.T.);
#17293=ADVANCED_FACE('',(#1958),#615,.F.);
#17294=ADVANCED_FACE('',(#1959),#16555,.F.);
#17295=ADVANCED_FACE('',(#1960),#409,.F.);
#17296=ADVANCED_FACE('',(#1961),#410,.F.);
#17297=ADVANCED_FACE('',(#1962),#16556,.T.);
#17298=ADVANCED_FACE('',(#1963),#616,.T.);
#17299=ADVANCED_FACE('',(#1964),#16557,.T.);
#17300=ADVANCED_FACE('',(#1965),#617,.T.);
#17301=ADVANCED_FACE('',(#1966),#16558,.T.);
#17302=ADVANCED_FACE('',(#1967),#16559,.F.);
#17303=ADVANCED_FACE('',(#1968,#925,#926),#16560,.F.);
#17304=ADVANCED_FACE('',(#1969),#16561,.F.);
#17305=ADVANCED_FACE('',(#1970),#16562,.F.);
#17306=ADVANCED_FACE('',(#1971),#16563,.F.);
#17307=ADVANCED_FACE('',(#1972),#16564,.T.);
#17308=ADVANCED_FACE('',(#1973),#16565,.T.);
#17309=ADVANCED_FACE('',(#1974),#16566,.F.);
#17310=ADVANCED_FACE('',(#1975),#618,.T.);
#17311=ADVANCED_FACE('',(#1976),#619,.F.);
#17312=ADVANCED_FACE('',(#1977),#620,.T.);
#17313=ADVANCED_FACE('',(#1978),#621,.F.);
#17314=ADVANCED_FACE('',(#1979),#16567,.T.);
#17315=ADVANCED_FACE('',(#1980),#16568,.F.);
#17316=ADVANCED_FACE('',(#1981),#16569,.T.);
#17317=ADVANCED_FACE('',(#1982),#16570,.F.);
#17318=ADVANCED_FACE('',(#1983),#16571,.T.);
#17319=ADVANCED_FACE('',(#1984),#16572,.F.);
#17320=ADVANCED_FACE('',(#1985),#16573,.F.);
#17321=ADVANCED_FACE('',(#1986),#16574,.F.);
#17322=ADVANCED_FACE('',(#1987),#16575,.F.);
#17323=ADVANCED_FACE('',(#1988),#16576,.F.);
#17324=ADVANCED_FACE('',(#1989),#16577,.F.);
#17325=ADVANCED_FACE('',(#1990),#16578,.F.);
#17326=ADVANCED_FACE('',(#1991),#16579,.F.);
#17327=ADVANCED_FACE('',(#1992),#16580,.F.);
#17328=ADVANCED_FACE('',(#1993),#16581,.F.);
#17329=ADVANCED_FACE('',(#1994),#16582,.F.);
#17330=ADVANCED_FACE('',(#1995),#16583,.F.);
#17331=ADVANCED_FACE('',(#1996),#622,.F.);
#17332=ADVANCED_FACE('',(#1997),#623,.F.);
#17333=ADVANCED_FACE('',(#1998),#624,.F.);
#17334=ADVANCED_FACE('',(#1999),#625,.F.);
#17335=ADVANCED_FACE('',(#2000),#626,.F.);
#17336=ADVANCED_FACE('',(#2001),#627,.F.);
#17337=ADVANCED_FACE('',(#2002),#628,.F.);
#17338=ADVANCED_FACE('',(#2003),#629,.F.);
#17339=ADVANCED_FACE('',(#2004),#630,.F.);
#17340=ADVANCED_FACE('',(#2005),#631,.F.);
#17341=ADVANCED_FACE('',(#2006),#632,.F.);
#17342=ADVANCED_FACE('',(#2007),#633,.F.);
#17343=ADVANCED_FACE('',(#2008),#634,.F.);
#17344=ADVANCED_FACE('',(#2009),#635,.F.);
#17345=ADVANCED_FACE('',(#2010),#636,.F.);
#17346=ADVANCED_FACE('',(#2011),#637,.F.);
#17347=ADVANCED_FACE('',(#2012),#638,.F.);
#17348=ADVANCED_FACE('',(#2013),#639,.F.);
#17349=ADVANCED_FACE('',(#2014),#640,.F.);
#17350=ADVANCED_FACE('',(#2015),#641,.T.);
#17351=ADVANCED_FACE('',(#2016),#642,.F.);
#17352=ADVANCED_FACE('',(#2017),#643,.F.);
#17353=ADVANCED_FACE('',(#2018),#644,.F.);
#17354=ADVANCED_FACE('',(#2019),#645,.F.);
#17355=ADVANCED_FACE('',(#2020),#646,.F.);
#17356=ADVANCED_FACE('',(#2021),#647,.F.);
#17357=ADVANCED_FACE('',(#2022),#648,.F.);
#17358=ADVANCED_FACE('',(#2023),#649,.F.);
#17359=ADVANCED_FACE('',(#2024),#650,.F.);
#17360=ADVANCED_FACE('',(#2025),#651,.F.);
#17361=ADVANCED_FACE('',(#2026),#652,.F.);
#17362=ADVANCED_FACE('',(#2027),#653,.F.);
#17363=ADVANCED_FACE('',(#2028),#654,.F.);
#17364=ADVANCED_FACE('',(#2029),#655,.F.);
#17365=ADVANCED_FACE('',(#2030),#656,.F.);
#17366=ADVANCED_FACE('',(#2031),#657,.F.);
#17367=ADVANCED_FACE('',(#2032),#658,.F.);
#17368=ADVANCED_FACE('',(#2033),#659,.F.);
#17369=ADVANCED_FACE('',(#2034),#660,.F.);
#17370=ADVANCED_FACE('',(#2035),#661,.F.);
#17371=ADVANCED_FACE('',(#2036),#662,.T.);
#17372=ADVANCED_FACE('',(#2037),#663,.T.);
#17373=ADVANCED_FACE('',(#2038),#664,.T.);
#17374=ADVANCED_FACE('',(#2039),#665,.T.);
#17375=ADVANCED_FACE('',(#2040),#666,.T.);
#17376=ADVANCED_FACE('',(#2041),#667,.T.);
#17377=ADVANCED_FACE('',(#2042),#668,.T.);
#17378=ADVANCED_FACE('',(#2043),#669,.T.);
#17379=ADVANCED_FACE('',(#2044),#670,.T.);
#17380=ADVANCED_FACE('',(#2045),#671,.T.);
#17381=ADVANCED_FACE('',(#2046),#672,.T.);
#17382=ADVANCED_FACE('',(#2047),#673,.F.);
#17383=ADVANCED_FACE('',(#2048),#674,.F.);
#17384=ADVANCED_FACE('',(#2049),#675,.F.);
#17385=ADVANCED_FACE('',(#2050),#676,.F.);
#17386=ADVANCED_FACE('',(#2051),#677,.F.);
#17387=ADVANCED_FACE('',(#2052),#16584,.F.);
#17388=ADVANCED_FACE('',(#2053),#16585,.F.);
#17389=ADVANCED_FACE('',(#2054),#16586,.F.);
#17390=ADVANCED_FACE('',(#2055),#16587,.F.);
#17391=ADVANCED_FACE('',(#2056),#16588,.T.);
#17392=ADVANCED_FACE('',(#2057),#16589,.F.);
#17393=ADVANCED_FACE('',(#2058),#16590,.F.);
#17394=ADVANCED_FACE('',(#2059),#16591,.F.);
#17395=ADVANCED_FACE('',(#2060),#16592,.T.);
#17396=ADVANCED_FACE('',(#2061),#16593,.F.);
#17397=ADVANCED_FACE('',(#2062),#16594,.F.);
#17398=ADVANCED_FACE('',(#2063),#16595,.F.);
#17399=ADVANCED_FACE('',(#2064),#16596,.T.);
#17400=ADVANCED_FACE('',(#2065),#16597,.F.);
#17401=ADVANCED_FACE('',(#2066),#16598,.F.);
#17402=ADVANCED_FACE('',(#2067),#16599,.F.);
#17403=ADVANCED_FACE('',(#2068),#678,.T.);
#17404=ADVANCED_FACE('',(#2069),#16600,.T.);
#17405=ADVANCED_FACE('',(#2070),#679,.T.);
#17406=ADVANCED_FACE('',(#2071,#927),#16601,.T.);
#17407=ADVANCED_FACE('',(#2072),#680,.F.);
#17408=ADVANCED_FACE('',(#2073),#227,.T.);
#17409=ADVANCED_FACE('',(#2074),#184,.T.);
#17410=ADVANCED_FACE('',(#2075),#681,.T.);
#17411=ADVANCED_FACE('',(#2076),#682,.T.);
#17412=ADVANCED_FACE('',(#2077),#683,.T.);
#17413=ADVANCED_FACE('',(#2078),#16602,.T.);
#17414=ADVANCED_FACE('',(#2079),#16603,.T.);
#17415=ADVANCED_FACE('',(#2080),#16604,.T.);
#17416=ADVANCED_FACE('',(#2081),#411,.T.);
#17417=ADVANCED_FACE('',(#2082),#412,.T.);
#17418=ADVANCED_FACE('',(#2083),#16605,.F.);
#17419=ADVANCED_FACE('',(#2084,#928),#16606,.T.);
#17420=ADVANCED_FACE('',(#2085),#684,.F.);
#17421=ADVANCED_FACE('',(#2086),#685,.F.);
#17422=ADVANCED_FACE('',(#2087),#686,.T.);
#17423=ADVANCED_FACE('',(#2088),#16607,.F.);
#17424=ADVANCED_FACE('',(#2089),#228,.T.);
#17425=ADVANCED_FACE('',(#2090),#229,.T.);
#17426=ADVANCED_FACE('',(#2091),#687,.F.);
#17427=ADVANCED_FACE('',(#2092),#688,.T.);
#17428=ADVANCED_FACE('',(#2093,#929),#16608,.T.);
#17429=ADVANCED_FACE('',(#2094,#930),#16609,.F.);
#17430=ADVANCED_FACE('',(#2095),#689,.T.);
#17431=ADVANCED_FACE('',(#2096,#931),#16610,.T.);
#17432=ADVANCED_FACE('',(#2097),#16611,.F.);
#17433=ADVANCED_FACE('',(#2098),#16612,.F.);
#17434=ADVANCED_FACE('',(#2099),#16613,.F.);
#17435=ADVANCED_FACE('',(#2100),#16614,.F.);
#17436=ADVANCED_FACE('',(#2101),#690,.F.);
#17437=ADVANCED_FACE('',(#2102),#691,.F.);
#17438=ADVANCED_FACE('',(#2103),#692,.F.);
#17439=ADVANCED_FACE('',(#2104),#693,.F.);
#17440=ADVANCED_FACE('',(#2105),#694,.F.);
#17441=ADVANCED_FACE('',(#2106),#16615,.F.);
#17442=ADVANCED_FACE('',(#2107),#16616,.F.);
#17443=ADVANCED_FACE('',(#2108),#16617,.F.);
#17444=ADVANCED_FACE('',(#2109),#16618,.F.);
#17445=ADVANCED_FACE('',(#2110),#16619,.F.);
#17446=ADVANCED_FACE('',(#2111),#16620,.F.);
#17447=ADVANCED_FACE('',(#2112),#16621,.F.);
#17448=ADVANCED_FACE('',(#2113),#16622,.F.);
#17449=ADVANCED_FACE('',(#2114),#16623,.F.);
#17450=ADVANCED_FACE('',(#2115),#16624,.F.);
#17451=ADVANCED_FACE('',(#2116),#16625,.F.);
#17452=ADVANCED_FACE('',(#2117),#16626,.F.);
#17453=ADVANCED_FACE('',(#2118),#16627,.F.);
#17454=ADVANCED_FACE('',(#2119),#16628,.F.);
#17455=ADVANCED_FACE('',(#2120),#16629,.F.);
#17456=ADVANCED_FACE('',(#2121),#16630,.F.);
#17457=ADVANCED_FACE('',(#2122),#16631,.F.);
#17458=ADVANCED_FACE('',(#2123),#16632,.F.);
#17459=ADVANCED_FACE('',(#2124),#16633,.F.);
#17460=ADVANCED_FACE('',(#2125),#16634,.F.);
#17461=ADVANCED_FACE('',(#2126),#16635,.F.);
#17462=ADVANCED_FACE('',(#2127),#16636,.F.);
#17463=ADVANCED_FACE('',(#2128),#16637,.F.);
#17464=ADVANCED_FACE('',(#2129),#16638,.F.);
#17465=ADVANCED_FACE('',(#2130),#16639,.F.);
#17466=ADVANCED_FACE('',(#2131),#16640,.F.);
#17467=ADVANCED_FACE('',(#2132),#16641,.F.);
#17468=ADVANCED_FACE('',(#2133),#16642,.F.);
#17469=ADVANCED_FACE('',(#2134),#16643,.F.);
#17470=ADVANCED_FACE('',(#2135),#16644,.F.);
#17471=ADVANCED_FACE('',(#2136),#16645,.F.);
#17472=ADVANCED_FACE('',(#2137),#16646,.F.);
#17473=ADVANCED_FACE('',(#2138),#16647,.F.);
#17474=ADVANCED_FACE('',(#2139),#16648,.F.);
#17475=ADVANCED_FACE('',(#2140),#16649,.F.);
#17476=ADVANCED_FACE('',(#2141),#16650,.F.);
#17477=ADVANCED_FACE('',(#2142),#16651,.F.);
#17478=ADVANCED_FACE('',(#2143),#16652,.F.);
#17479=ADVANCED_FACE('',(#2144),#16653,.F.);
#17480=ADVANCED_FACE('',(#2145),#16654,.F.);
#17481=ADVANCED_FACE('',(#2146),#16655,.F.);
#17482=ADVANCED_FACE('',(#2147),#16656,.F.);
#17483=ADVANCED_FACE('',(#2148),#16657,.F.);
#17484=ADVANCED_FACE('',(#2149),#16658,.F.);
#17485=ADVANCED_FACE('',(#2150),#16659,.F.);
#17486=ADVANCED_FACE('',(#2151),#16660,.F.);
#17487=ADVANCED_FACE('',(#2152),#16661,.F.);
#17488=ADVANCED_FACE('',(#2153),#16662,.F.);
#17489=ADVANCED_FACE('',(#2154),#16663,.F.);
#17490=ADVANCED_FACE('',(#2155),#16664,.F.);
#17491=ADVANCED_FACE('',(#2156),#16665,.F.);
#17492=ADVANCED_FACE('',(#2157),#16666,.F.);
#17493=ADVANCED_FACE('',(#2158),#16667,.F.);
#17494=ADVANCED_FACE('',(#2159),#16668,.F.);
#17495=ADVANCED_FACE('',(#2160),#16669,.F.);
#17496=ADVANCED_FACE('',(#2161),#16670,.F.);
#17497=ADVANCED_FACE('',(#2162),#16671,.F.);
#17498=ADVANCED_FACE('',(#2163),#16672,.F.);
#17499=ADVANCED_FACE('',(#2164),#16673,.F.);
#17500=ADVANCED_FACE('',(#2165),#16674,.F.);
#17501=ADVANCED_FACE('',(#2166),#16675,.F.);
#17502=ADVANCED_FACE('',(#2167),#16676,.F.);
#17503=ADVANCED_FACE('',(#2168),#16677,.F.);
#17504=ADVANCED_FACE('',(#2169),#16678,.F.);
#17505=ADVANCED_FACE('',(#2170),#16679,.F.);
#17506=ADVANCED_FACE('',(#2171),#16680,.F.);
#17507=ADVANCED_FACE('',(#2172),#16681,.F.);
#17508=ADVANCED_FACE('',(#2173),#16682,.F.);
#17509=ADVANCED_FACE('',(#2174),#16683,.F.);
#17510=ADVANCED_FACE('',(#2175),#16684,.F.);
#17511=ADVANCED_FACE('',(#2176),#16685,.F.);
#17512=ADVANCED_FACE('',(#2177),#16686,.F.);
#17513=ADVANCED_FACE('',(#2178),#16687,.F.);
#17514=ADVANCED_FACE('',(#2179),#16688,.F.);
#17515=ADVANCED_FACE('',(#2180),#16689,.F.);
#17516=ADVANCED_FACE('',(#2181),#16690,.F.);
#17517=ADVANCED_FACE('',(#2182),#16691,.F.);
#17518=ADVANCED_FACE('',(#2183),#16692,.F.);
#17519=ADVANCED_FACE('',(#2184),#16693,.F.);
#17520=ADVANCED_FACE('',(#2185),#16694,.F.);
#17521=ADVANCED_FACE('',(#2186),#16695,.F.);
#17522=ADVANCED_FACE('',(#2187),#16696,.F.);
#17523=ADVANCED_FACE('',(#2188),#16697,.F.);
#17524=ADVANCED_FACE('',(#2189),#16698,.F.);
#17525=ADVANCED_FACE('',(#2190),#16699,.F.);
#17526=ADVANCED_FACE('',(#2191),#16700,.F.);
#17527=ADVANCED_FACE('',(#2192),#16701,.F.);
#17528=ADVANCED_FACE('',(#2193),#16702,.F.);
#17529=ADVANCED_FACE('',(#2194),#16703,.F.);
#17530=ADVANCED_FACE('',(#2195),#16704,.F.);
#17531=ADVANCED_FACE('',(#2196,#932,#933,#934,#935,#936),#16705,.T.);
#17532=ADVANCED_FACE('',(#2197,#937),#16706,.F.);
#17533=ADVANCED_FACE('',(#2198),#695,.T.);
#17534=ADVANCED_FACE('',(#2199,#938),#16707,.F.);
#17535=ADVANCED_FACE('',(#2200,#939),#16708,.T.);
#17536=ADVANCED_FACE('',(#2201),#696,.T.);
#17537=ADVANCED_FACE('',(#2202),#413,.F.);
#17538=ADVANCED_FACE('',(#2203),#697,.F.);
#17539=ADVANCED_FACE('',(#2204),#414,.F.);
#17540=ADVANCED_FACE('',(#2205),#16709,.T.);
#17541=ADVANCED_FACE('',(#2206),#16710,.T.);
#17542=ADVANCED_FACE('',(#2207),#698,.T.);
#17543=ADVANCED_FACE('',(#2208),#699,.T.);
#17544=ADVANCED_FACE('',(#2209),#185,.F.);
#17545=ADVANCED_FACE('',(#2210),#186,.F.);
#17546=ADVANCED_FACE('',(#2211),#187,.T.);
#17547=ADVANCED_FACE('',(#2212),#188,.T.);
#17548=ADVANCED_FACE('',(#2213),#700,.T.);
#17549=ADVANCED_FACE('',(#2214,#940),#16711,.F.);
#17550=ADVANCED_FACE('',(#2215,#941),#16712,.T.);
#17551=ADVANCED_FACE('',(#2216),#701,.F.);
#17552=ADVANCED_FACE('',(#2217),#702,.F.);
#17553=ADVANCED_FACE('',(#2218),#16713,.T.);
#17554=ADVANCED_FACE('',(#2219),#703,.F.);
#17555=ADVANCED_FACE('',(#2220),#16714,.F.);
#17556=ADVANCED_FACE('',(#2221),#16715,.T.);
#17557=ADVANCED_FACE('',(#2222),#16716,.T.);
#17558=ADVANCED_FACE('',(#2223),#16717,.T.);
#17559=ADVANCED_FACE('',(#2224),#16718,.T.);
#17560=ADVANCED_FACE('',(#2225),#16719,.T.);
#17561=ADVANCED_FACE('',(#2226),#16720,.T.);
#17562=ADVANCED_FACE('',(#2227),#16721,.F.);
#17563=ADVANCED_FACE('',(#2228),#53,.T.);
#17564=ADVANCED_FACE('',(#2229),#54,.T.);
#17565=ADVANCED_FACE('',(#2230),#16722,.T.);
#17566=ADVANCED_FACE('',(#2231),#16723,.T.);
#17567=ADVANCED_FACE('',(#2232),#16724,.T.);
#17568=ADVANCED_FACE('',(#2233),#16725,.T.);
#17569=ADVANCED_FACE('',(#2234),#16726,.T.);
#17570=ADVANCED_FACE('',(#2235),#55,.T.);
#17571=ADVANCED_FACE('',(#2236),#56,.T.);
#17572=ADVANCED_FACE('',(#2237),#57,.T.);
#17573=ADVANCED_FACE('',(#2238),#16727,.T.);
#17574=ADVANCED_FACE('',(#2239),#58,.T.);
#17575=ADVANCED_FACE('',(#2240),#16728,.F.);
#17576=ADVANCED_FACE('',(#2241),#16729,.F.);
#17577=ADVANCED_FACE('',(#2242),#16730,.F.);
#17578=ADVANCED_FACE('',(#2243),#16731,.F.);
#17579=ADVANCED_FACE('',(#2244),#16732,.F.);
#17580=ADVANCED_FACE('',(#2245),#16733,.F.);
#17581=ADVANCED_FACE('',(#2246),#16734,.F.);
#17582=ADVANCED_FACE('',(#2247),#16735,.F.);
#17583=ADVANCED_FACE('',(#2248),#16736,.F.);
#17584=ADVANCED_FACE('',(#2249),#16737,.F.);
#17585=ADVANCED_FACE('',(#2250),#704,.F.);
#17586=ADVANCED_FACE('',(#2251),#705,.F.);
#17587=ADVANCED_FACE('',(#2252),#16738,.F.);
#17588=ADVANCED_FACE('',(#2253),#16739,.F.);
#17589=ADVANCED_FACE('',(#2254),#16740,.F.);
#17590=ADVANCED_FACE('',(#2255),#16741,.F.);
#17591=ADVANCED_FACE('',(#2256,#942,#943),#16742,.F.);
#17592=ADVANCED_FACE('',(#2257),#16743,.T.);
#17593=ADVANCED_FACE('',(#2258,#944,#945),#16744,.F.);
#17594=ADVANCED_FACE('',(#2259,#946,#947),#16745,.T.);
#17595=ADVANCED_FACE('',(#2260),#16746,.F.);
#17596=ADVANCED_FACE('',(#2261),#706,.F.);
#17597=ADVANCED_FACE('',(#2262),#707,.F.);
#17598=ADVANCED_FACE('',(#2263,#948),#16747,.F.);
#17599=ADVANCED_FACE('',(#2264),#16748,.F.);
#17600=ADVANCED_FACE('',(#2265),#16749,.F.);
#17601=ADVANCED_FACE('',(#2266,#949),#16750,.F.);
#17602=ADVANCED_FACE('',(#2267,#950),#16751,.F.);
#17603=ADVANCED_FACE('',(#2268),#708,.F.);
#17604=ADVANCED_FACE('',(#2269),#709,.F.);
#17605=ADVANCED_FACE('',(#2270),#16752,.F.);
#17606=ADVANCED_FACE('',(#2271),#16753,.F.);
#17607=ADVANCED_FACE('',(#2272),#16754,.F.);
#17608=ADVANCED_FACE('',(#2273),#16755,.F.);
#17609=ADVANCED_FACE('',(#2274,#951,#952),#16756,.F.);
#17610=ADVANCED_FACE('',(#2275),#16757,.F.);
#17611=ADVANCED_FACE('',(#2276),#16758,.T.);
#17612=ADVANCED_FACE('',(#2277),#16759,.F.);
#17613=ADVANCED_FACE('',(#2278,#953),#16760,.F.);
#17614=ADVANCED_FACE('',(#2279),#16761,.F.);
#17615=ADVANCED_FACE('',(#2280),#16762,.F.);
#17616=ADVANCED_FACE('',(#2281),#16763,.F.);
#17617=ADVANCED_FACE('',(#2282),#16764,.F.);
#17618=ADVANCED_FACE('',(#2283),#16765,.T.);
#17619=ADVANCED_FACE('',(#2284),#16766,.F.);
#17620=ADVANCED_FACE('',(#2285),#16767,.F.);
#17621=ADVANCED_FACE('',(#2286,#954,#955),#16768,.F.);
#17622=ADVANCED_FACE('',(#2287,#956),#16769,.T.);
#17623=ADVANCED_FACE('',(#2288),#189,.T.);
#17624=ADVANCED_FACE('',(#2289),#710,.F.);
#17625=ADVANCED_FACE('',(#2290),#711,.F.);
#17626=ADVANCED_FACE('',(#2291),#712,.F.);
#17627=ADVANCED_FACE('',(#2292),#713,.F.);
#17628=ADVANCED_FACE('',(#2293),#714,.F.);
#17629=ADVANCED_FACE('',(#2294),#715,.F.);
#17630=ADVANCED_FACE('',(#2295),#716,.F.);
#17631=ADVANCED_FACE('',(#2296),#717,.F.);
#17632=ADVANCED_FACE('',(#2297),#718,.F.);
#17633=ADVANCED_FACE('',(#2298),#719,.F.);
#17634=ADVANCED_FACE('',(#2299),#720,.F.);
#17635=ADVANCED_FACE('',(#2300),#721,.F.);
#17636=ADVANCED_FACE('',(#2301),#722,.F.);
#17637=ADVANCED_FACE('',(#2302),#723,.F.);
#17638=ADVANCED_FACE('',(#2303),#724,.F.);
#17639=ADVANCED_FACE('',(#2304),#725,.F.);
#17640=ADVANCED_FACE('',(#2305),#726,.F.);
#17641=ADVANCED_FACE('',(#2306),#727,.F.);
#17642=ADVANCED_FACE('',(#2307),#728,.F.);
#17643=ADVANCED_FACE('',(#2308),#729,.F.);
#17644=ADVANCED_FACE('',(#2309),#730,.F.);
#17645=ADVANCED_FACE('',(#2310),#731,.F.);
#17646=ADVANCED_FACE('',(#2311),#732,.F.);
#17647=ADVANCED_FACE('',(#2312),#733,.F.);
#17648=ADVANCED_FACE('',(#2313),#734,.F.);
#17649=ADVANCED_FACE('',(#2314),#735,.F.);
#17650=ADVANCED_FACE('',(#2315),#736,.F.);
#17651=ADVANCED_FACE('',(#2316),#737,.F.);
#17652=ADVANCED_FACE('',(#2317),#738,.F.);
#17653=ADVANCED_FACE('',(#2318),#739,.T.);
#17654=ADVANCED_FACE('',(#2319),#740,.T.);
#17655=ADVANCED_FACE('',(#2320),#741,.T.);
#17656=ADVANCED_FACE('',(#2321),#230,.T.);
#17657=ADVANCED_FACE('',(#2322),#231,.T.);
#17658=ADVANCED_FACE('',(#2323),#232,.T.);
#17659=ADVANCED_FACE('',(#2324),#233,.T.);
#17660=ADVANCED_FACE('',(#2325),#742,.F.);
#17661=ADVANCED_FACE('',(#2326),#743,.T.);
#17662=ADVANCED_FACE('',(#2327,#957),#16770,.F.);
#17663=ADVANCED_FACE('',(#2328,#958),#16771,.T.);
#17664=ADVANCED_FACE('',(#2329,#959),#16772,.F.);
#17665=ADVANCED_FACE('',(#2330),#744,.T.);
#17666=ADVANCED_FACE('',(#2331),#415,.T.);
#17667=ADVANCED_FACE('',(#2332),#745,.F.);
#17668=ADVANCED_FACE('',(#2333),#416,.T.);
#17669=ADVANCED_FACE('',(#2334),#16773,.F.);
#17670=ADVANCED_FACE('',(#2335),#16774,.F.);
#17671=ADVANCED_FACE('',(#2336),#746,.T.);
#17672=ADVANCED_FACE('',(#2337),#190,.F.);
#17673=ADVANCED_FACE('',(#2338),#191,.F.);
#17674=ADVANCED_FACE('',(#2339),#192,.T.);
#17675=ADVANCED_FACE('',(#2340,#960),#16775,.T.);
#17676=ADVANCED_FACE('',(#2341),#747,.F.);
#17677=ADVANCED_FACE('',(#2342),#16776,.F.);
#17678=ADVANCED_FACE('',(#2343),#234,.T.);
#17679=ADVANCED_FACE('',(#2344),#235,.T.);
#17680=ADVANCED_FACE('',(#2345),#748,.T.);
#17681=ADVANCED_FACE('',(#2346),#749,.T.);
#17682=ADVANCED_FACE('',(#2347),#750,.T.);
#17683=ADVANCED_FACE('',(#2348),#751,.T.);
#17684=ADVANCED_FACE('',(#2349,#961,#962),#16777,.T.);
#17685=ADVANCED_FACE('',(#2350),#752,.T.);
#17686=ADVANCED_FACE('',(#2351,#963,#964),#16778,.F.);
#17687=ADVANCED_FACE('',(#2352),#16779,.F.);
#17688=ADVANCED_FACE('',(#2353),#16780,.F.);
#17689=ADVANCED_FACE('',(#2354),#16781,.F.);
#17690=ADVANCED_FACE('',(#2355),#16782,.F.);
#17691=ADVANCED_FACE('',(#2356),#16783,.F.);
#17692=ADVANCED_FACE('',(#2357),#753,.T.);
#17693=ADVANCED_FACE('',(#2358),#16784,.F.);
#17694=ADVANCED_FACE('',(#2359),#16785,.F.);
#17695=ADVANCED_FACE('',(#2360),#16786,.F.);
#17696=ADVANCED_FACE('',(#2361),#16787,.F.);
#17697=ADVANCED_FACE('',(#2362),#16788,.F.);
#17698=ADVANCED_FACE('',(#2363),#16789,.F.);
#17699=ADVANCED_FACE('',(#2364),#16790,.T.);
#17700=ADVANCED_FACE('',(#2365),#16791,.F.);
#17701=ADVANCED_FACE('',(#2366),#16792,.F.);
#17702=ADVANCED_FACE('',(#2367,#965),#16793,.F.);
#17703=ADVANCED_FACE('',(#2368),#754,.F.);
#17704=ADVANCED_FACE('',(#2369),#755,.T.);
#17705=ADVANCED_FACE('',(#2370),#756,.F.);
#17706=ADVANCED_FACE('',(#2371),#757,.T.);
#17707=ADVANCED_FACE('',(#2372),#16794,.T.);
#17708=ADVANCED_FACE('',(#2373),#16795,.F.);
#17709=ADVANCED_FACE('',(#2374),#16796,.F.);
#17710=ADVANCED_FACE('',(#2375,#966),#16797,.T.);
#17711=ADVANCED_FACE('',(#2376),#758,.T.);
#17712=ADVANCED_FACE('',(#2377),#759,.F.);
#17713=ADVANCED_FACE('',(#2378),#760,.F.);
#17714=ADVANCED_FACE('',(#2379),#761,.T.);
#17715=ADVANCED_FACE('',(#2380,#967),#16798,.F.);
#17716=ADVANCED_FACE('',(#2381),#16799,.T.);
#17717=ADVANCED_FACE('',(#2382),#16800,.T.);
#17718=ADVANCED_FACE('',(#2383),#16801,.T.);
#17719=ADVANCED_FACE('',(#2384),#16802,.T.);
#17720=ADVANCED_FACE('',(#2385),#16803,.T.);
#17721=ADVANCED_FACE('',(#2386),#16804,.T.);
#17722=ADVANCED_FACE('',(#2387),#16805,.T.);
#17723=ADVANCED_FACE('',(#2388),#16806,.F.);
#17724=ADVANCED_FACE('',(#2389),#762,.T.);
#17725=ADVANCED_FACE('',(#2390),#763,.T.);
#17726=ADVANCED_FACE('',(#2391),#764,.T.);
#17727=ADVANCED_FACE('',(#2392),#765,.T.);
#17728=ADVANCED_FACE('',(#2393),#766,.T.);
#17729=ADVANCED_FACE('',(#2394),#767,.T.);
#17730=ADVANCED_FACE('',(#2395),#768,.F.);
#17731=ADVANCED_FACE('',(#2396,#968),#16807,.F.);
#17732=ADVANCED_FACE('',(#2397),#769,.F.);
#17733=ADVANCED_FACE('',(#2398),#16808,.F.);
#17734=ADVANCED_FACE('',(#2399),#770,.T.);
#17735=ADVANCED_FACE('',(#2400),#16809,.F.);
#17736=ADVANCED_FACE('',(#2401),#16810,.F.);
#17737=ADVANCED_FACE('',(#2402),#16811,.F.);
#17738=ADVANCED_FACE('',(#2403),#16812,.F.);
#17739=ADVANCED_FACE('',(#2404),#16813,.F.);
#17740=ADVANCED_FACE('',(#2405),#16814,.F.);
#17741=ADVANCED_FACE('',(#2406),#16815,.F.);
#17742=ADVANCED_FACE('',(#2407),#16816,.F.);
#17743=ADVANCED_FACE('',(#2408),#16817,.F.);
#17744=ADVANCED_FACE('',(#2409),#16818,.F.);
#17745=ADVANCED_FACE('',(#2410),#16819,.F.);
#17746=ADVANCED_FACE('',(#2411),#16820,.F.);
#17747=ADVANCED_FACE('',(#2412),#16821,.F.);
#17748=ADVANCED_FACE('',(#2413),#16822,.F.);
#17749=ADVANCED_FACE('',(#2414),#16823,.F.);
#17750=ADVANCED_FACE('',(#2415),#16824,.F.);
#17751=ADVANCED_FACE('',(#2416),#16825,.F.);
#17752=ADVANCED_FACE('',(#2417),#16826,.F.);
#17753=ADVANCED_FACE('',(#2418),#16827,.F.);
#17754=ADVANCED_FACE('',(#2419),#16828,.F.);
#17755=ADVANCED_FACE('',(#2420),#16829,.F.);
#17756=ADVANCED_FACE('',(#2421),#16830,.F.);
#17757=ADVANCED_FACE('',(#2422),#16831,.F.);
#17758=ADVANCED_FACE('',(#2423),#16832,.F.);
#17759=ADVANCED_FACE('',(#2424),#16833,.F.);
#17760=ADVANCED_FACE('',(#2425),#16834,.F.);
#17761=ADVANCED_FACE('',(#2426),#16835,.F.);
#17762=ADVANCED_FACE('',(#2427),#16836,.F.);
#17763=ADVANCED_FACE('',(#2428),#16837,.F.);
#17764=ADVANCED_FACE('',(#2429),#16838,.F.);
#17765=ADVANCED_FACE('',(#2430),#16839,.F.);
#17766=ADVANCED_FACE('',(#2431),#16840,.F.);
#17767=ADVANCED_FACE('',(#2432),#16841,.F.);
#17768=ADVANCED_FACE('',(#2433),#16842,.F.);
#17769=ADVANCED_FACE('',(#2434),#16843,.F.);
#17770=ADVANCED_FACE('',(#2435),#16844,.F.);
#17771=ADVANCED_FACE('',(#2436),#16845,.F.);
#17772=ADVANCED_FACE('',(#2437),#16846,.F.);
#17773=ADVANCED_FACE('',(#2438),#771,.T.);
#17774=ADVANCED_FACE('',(#2439),#16847,.F.);
#17775=ADVANCED_FACE('',(#2440),#16848,.F.);
#17776=ADVANCED_FACE('',(#2441,#969),#16849,.F.);
#17777=ADVANCED_FACE('',(#2442,#970),#16850,.T.);
#17778=ADVANCED_FACE('',(#2443),#16851,.T.);
#17779=ADVANCED_FACE('',(#2444),#772,.F.);
#17780=ADVANCED_FACE('',(#2445),#16852,.F.);
#17781=ADVANCED_FACE('',(#2446),#773,.T.);
#17782=ADVANCED_FACE('',(#2447),#16853,.F.);
#17783=ADVANCED_FACE('',(#2448),#16854,.F.);
#17784=ADVANCED_FACE('',(#2449),#16855,.F.);
#17785=ADVANCED_FACE('',(#2450),#16856,.F.);
#17786=ADVANCED_FACE('',(#2451),#774,.T.);
#17787=ADVANCED_FACE('',(#2452),#16857,.F.);
#17788=ADVANCED_FACE('',(#2453),#16858,.F.);
#17789=ADVANCED_FACE('',(#2454),#16859,.F.);
#17790=ADVANCED_FACE('',(#2455),#775,.T.);
#17791=ADVANCED_FACE('',(#2456,#971),#16860,.T.);
#17792=ADVANCED_FACE('',(#2457,#972),#16861,.F.);
#17793=CLOSED_SHELL('',(#16862,#16863,#16864,#16865,#16866,#16867,#16868,
#16869,#16870,#16871,#16872,#16873,#16874,#16875,#16876,#16877,#16878,#16879,
#16880,#16881,#16882,#16883,#16884,#16885,#16886,#16887,#16888,#16889,#16890,
#16891,#16892,#16893,#16894,#16895,#16896,#16897,#16898,#16899,#16900,#16901,
#16902,#16903,#16904,#16905,#16906,#16907,#16908,#16909,#16910,#16911,#16912,
#16913,#16914,#16915,#16916,#16917,#16918,#16919,#16920,#16921,#16922,#16923,
#16924,#16925,#16926,#16927,#16928,#16929,#16930,#16931,#16932,#16933,#16934,
#16935,#16936,#16937,#16938,#16939,#16940,#16941,#16942,#16943,#16944,#16945,
#16946,#16947,#16948,#16949,#16950,#16951,#16952,#16953,#16954,#16955,#16956,
#16957,#16958,#16959,#16960,#16961,#16962,#16963,#16964,#16965,#16966,#16967,
#16968,#16969,#16970,#16971,#16972,#16973,#16974,#16975,#16976,#16977,#16978,
#16979,#16980,#16981,#16982,#16983,#16984,#16985,#16986,#16987,#16988,#16989,
#16990,#16991,#16992,#16993,#16994,#16995,#16996,#16997));
#17794=CLOSED_SHELL('',(#16998,#16999,#17000,#17001,#17002,#17003,#17004,
#17005,#17006,#17007,#17008,#17009,#17010,#17011,#17012,#17013,#17014,#17015,
#17016,#17017,#17018,#17019,#17020,#17021,#17022,#17023,#17024,#17025,#17026,
#17027,#17028,#17029,#17030,#17031,#17032,#17033,#17034,#17035,#17036,#17037,
#17038,#17039,#17040,#17041,#17042,#17043,#17044,#17045,#17046,#17047,#17048,
#17049,#17050,#17051,#17052,#17053,#17054,#17055,#17056,#17057,#17058,#17059,
#17060,#17061,#17062,#17063,#17064,#17065,#17066,#17067,#17068,#17069,#17070,
#17071,#17072,#17073,#17074,#17075,#17076,#17077,#17078,#17079,#17080,#17081,
#17082,#17083,#17084,#17085,#17086,#17087,#17088,#17089,#17090,#17091,#17092,
#17093));
#17795=CLOSED_SHELL('',(#17094,#17095,#17096,#17097,#17098,#17099,#17100,
#17101,#17102,#17103,#17104,#17105,#17106,#17107,#17108,#17109,#17110,#17111,
#17112,#17113,#17114,#17115,#17116,#17117,#17118,#17119,#17120,#17121,#17122,
#17123,#17124,#17125,#17126,#17127,#17128,#17129,#17130,#17131,#17132,#17133,
#17134,#17135,#17136,#17137,#17138,#17139,#17140,#17141,#17142,#17143,#17144,
#17145,#17146,#17147,#17148,#17149,#17150,#17151,#17152,#17153,#17154,#17155,
#17156,#17157,#17158,#17159,#17160,#17161,#17162,#17163,#17164,#17165,#17166,
#17167,#17168,#17169,#17170,#17171,#17172,#17173,#17174,#17175,#17176,#17177,
#17178,#17179,#17180,#17181,#17182,#17183,#17184,#17185,#17186,#17187,#17188,
#17189,#17190,#17191,#17192,#17193,#17194,#17195,#17196,#17197,#17198,#17199,
#17200,#17201,#17202,#17203,#17204,#17205,#17206,#17207,#17208,#17209,#17210,
#17211,#17212,#17213,#17214));
#17796=CLOSED_SHELL('',(#17215,#17216,#17217,#17218,#17219,#17220,#17221,
#17222,#17223,#17224,#17225,#17226,#17227,#17228,#17229,#17230,#17231,#17232,
#17233,#17234,#17235,#17236,#17237,#17238,#17239,#17240,#17241,#17242,#17243,
#17244,#17245,#17246,#17247,#17248,#17249,#17250,#17251,#17252,#17253,#17254,
#17255,#17256,#17257,#17258,#17259,#17260,#17261,#17262,#17263,#17264,#17265,
#17266,#17267,#17268,#17269,#17270,#17271,#17272,#17273,#17274,#17275,#17276,
#17277,#17278,#17279,#17280,#17281,#17282,#17283,#17284,#17285,#17286,#17287,
#17288,#17289,#17290,#17291));
#17797=CLOSED_SHELL('',(#17292,#17293,#17294,#17295,#17296,#17297,#17298,
#17299,#17300,#17301,#17302,#17303,#17304,#17305,#17306,#17307));
#17798=CLOSED_SHELL('',(#17308,#17309,#17310,#17311,#17312,#17313,#17314,
#17315,#17316,#17317,#17318,#17319,#17320,#17321,#17322,#17323,#17324,#17325,
#17326,#17327,#17328,#17329,#17330));
#17799=CLOSED_SHELL('',(#17331,#17332,#17333,#17334,#17335,#17336,#17337,
#17338,#17339,#17340,#17341,#17342,#17343,#17344,#17345,#17346,#17347,#17348,
#17349,#17350,#17351,#17352,#17353,#17354,#17355,#17356,#17357,#17358,#17359,
#17360,#17361,#17362,#17363,#17364,#17365,#17366,#17367,#17368,#17369,#17370,
#17371,#17372,#17373,#17374,#17375,#17376,#17377,#17378,#17379,#17380,#17381,
#17382,#17383,#17384,#17385,#17386,#17387,#17388,#17389,#17390,#17391,#17392,
#17393,#17394,#17395,#17396,#17397,#17398,#17399,#17400,#17401,#17402,#17403,
#17404,#17405,#17406,#17407,#17408,#17409,#17410,#17411,#17412,#17413,#17414,
#17415,#17416,#17417,#17418,#17419,#17420,#17421,#17422,#17423,#17424,#17425,
#17426,#17427,#17428,#17429,#17430,#17431,#17432,#17433,#17434,#17435,#17436,
#17437,#17438,#17439,#17440,#17441,#17442,#17443,#17444,#17445,#17446,#17447,
#17448,#17449,#17450,#17451,#17452,#17453,#17454,#17455,#17456,#17457,#17458,
#17459,#17460,#17461,#17462,#17463,#17464,#17465,#17466,#17467,#17468,#17469,
#17470,#17471,#17472,#17473,#17474,#17475,#17476,#17477,#17478,#17479,#17480,
#17481,#17482,#17483,#17484,#17485,#17486,#17487,#17488,#17489,#17490,#17491,
#17492,#17493,#17494,#17495,#17496,#17497,#17498,#17499,#17500,#17501,#17502,
#17503,#17504,#17505,#17506,#17507,#17508,#17509,#17510,#17511,#17512,#17513,
#17514,#17515,#17516,#17517,#17518,#17519,#17520,#17521,#17522,#17523,#17524,
#17525,#17526,#17527,#17528,#17529,#17530,#17531,#17532,#17533,#17534,#17535,
#17536,#17537,#17538,#17539,#17540,#17541,#17542,#17543,#17544,#17545,#17546,
#17547,#17548,#17549,#17550,#17551));
#17800=CLOSED_SHELL('',(#17552,#17553,#17554,#17555,#17556,#17557,#17558,
#17559,#17560,#17561,#17562,#17563,#17564,#17565,#17566,#17567,#17568,#17569,
#17570,#17571,#17572,#17573,#17574,#17575,#17576,#17577,#17578,#17579,#17580,
#17581,#17582,#17583,#17584,#17585,#17586,#17587,#17588,#17589,#17590,#17591,
#17592,#17593,#17594,#17595,#17596,#17597,#17598,#17599,#17600,#17601,#17602,
#17603,#17604,#17605,#17606,#17607,#17608,#17609,#17610,#17611,#17612,#17613,
#17614,#17615,#17616,#17617,#17618,#17619,#17620,#17621));
#17801=CLOSED_SHELL('',(#17622,#17623,#17624));
#17802=CLOSED_SHELL('',(#17625,#17626,#17627,#17628,#17629,#17630,#17631,
#17632,#17633,#17634,#17635,#17636,#17637,#17638,#17639,#17640,#17641,#17642,
#17643,#17644,#17645,#17646,#17647,#17648,#17649,#17650,#17651,#17652,#17653,
#17654,#17655,#17656,#17657,#17658,#17659,#17660,#17661,#17662,#17663,#17664,
#17665,#17666,#17667,#17668,#17669,#17670,#17671,#17672,#17673,#17674,#17675,
#17676,#17677,#17678,#17679,#17680,#17681,#17682,#17683,#17684,#17685,#17686,
#17687,#17688,#17689,#17690,#17691,#17692,#17693,#17694,#17695,#17696,#17697,
#17698,#17699,#17700,#17701,#17702,#17703,#17704,#17705,#17706,#17707,#17708,
#17709,#17710,#17711,#17712,#17713,#17714,#17715,#17716,#17717,#17718,#17719,
#17720,#17721,#17722,#17723,#17724,#17725,#17726,#17727,#17728,#17729,#17730,
#17731,#17732,#17733,#17734,#17735,#17736,#17737,#17738,#17739,#17740,#17741,
#17742,#17743,#17744,#17745,#17746,#17747,#17748,#17749,#17750,#17751,#17752,
#17753,#17754,#17755,#17756,#17757,#17758,#17759,#17760,#17761,#17762,#17763,
#17764,#17765,#17766,#17767,#17768,#17769,#17770,#17771,#17772,#17773,#17774,
#17775,#17776,#17777,#17778));
#17803=CLOSED_SHELL('',(#17779,#17780,#17781,#17782,#17783,#17784,#17785,
#17786,#17787,#17788,#17789,#17790,#17791,#17792));
#17804=DERIVED_UNIT_ELEMENT(#17824,1.);
#17805=DERIVED_UNIT_ELEMENT(#36670,-3.);
#17806=DERIVED_UNIT_ELEMENT(#17824,1.);
#17807=DERIVED_UNIT_ELEMENT(#36670,-3.);
#17808=DERIVED_UNIT_ELEMENT(#17824,1.);
#17809=DERIVED_UNIT_ELEMENT(#36670,-3.);
#17810=DERIVED_UNIT_ELEMENT(#17824,1.);
#17811=DERIVED_UNIT_ELEMENT(#36670,-3.);
#17812=DERIVED_UNIT_ELEMENT(#17824,1.);
#17813=DERIVED_UNIT_ELEMENT(#36670,-3.);
#17814=DERIVED_UNIT_ELEMENT(#17824,1.);
#17815=DERIVED_UNIT_ELEMENT(#36670,-3.);
#17816=DERIVED_UNIT_ELEMENT(#17824,1.);
#17817=DERIVED_UNIT_ELEMENT(#36670,-3.);
#17818=DERIVED_UNIT_ELEMENT(#17824,1.);
#17819=DERIVED_UNIT_ELEMENT(#36670,-3.);
#17820=DERIVED_UNIT_ELEMENT(#17824,1.);
#17821=DERIVED_UNIT_ELEMENT(#36670,-3.);
#17822=DERIVED_UNIT_ELEMENT(#17824,1.);
#17823=DERIVED_UNIT_ELEMENT(#36670,-3.);
#17824=(
MASS_UNIT()
NAMED_UNIT(*)
SI_UNIT(.KILO.,.GRAM.)
);
#17825=DERIVED_UNIT((#17804,#17805));
#17826=DERIVED_UNIT((#17806,#17807));
#17827=DERIVED_UNIT((#17808,#17809));
#17828=DERIVED_UNIT((#17810,#17811));
#17829=DERIVED_UNIT((#17812,#17813));
#17830=DERIVED_UNIT((#17814,#17815));
#17831=DERIVED_UNIT((#17816,#17817));
#17832=DERIVED_UNIT((#17818,#17819));
#17833=DERIVED_UNIT((#17820,#17821));
#17834=DERIVED_UNIT((#17822,#17823));
#17835=MEASURE_REPRESENTATION_ITEM('density measure',
POSITIVE_RATIO_MEASURE(7850.),#17825);
#17836=MEASURE_REPRESENTATION_ITEM('density measure',
POSITIVE_RATIO_MEASURE(7850.),#17826);
#17837=MEASURE_REPRESENTATION_ITEM('density measure',
POSITIVE_RATIO_MEASURE(7850.),#17827);
#17838=MEASURE_REPRESENTATION_ITEM('density measure',
POSITIVE_RATIO_MEASURE(7850.),#17828);
#17839=MEASURE_REPRESENTATION_ITEM('density measure',
POSITIVE_RATIO_MEASURE(7850.),#17829);
#17840=MEASURE_REPRESENTATION_ITEM('density measure',
POSITIVE_RATIO_MEASURE(7850.),#17830);
#17841=MEASURE_REPRESENTATION_ITEM('density measure',
POSITIVE_RATIO_MEASURE(7850.),#17831);
#17842=MEASURE_REPRESENTATION_ITEM('density measure',
POSITIVE_RATIO_MEASURE(7850.),#17832);
#17843=MEASURE_REPRESENTATION_ITEM('density measure',
POSITIVE_RATIO_MEASURE(7850.),#17833);
#17844=MEASURE_REPRESENTATION_ITEM('density measure',
POSITIVE_RATIO_MEASURE(7850.),#17834);
#17845=PROPERTY_DEFINITION_REPRESENTATION(#17895,#17865);
#17846=PROPERTY_DEFINITION_REPRESENTATION(#17896,#17866);
#17847=PROPERTY_DEFINITION_REPRESENTATION(#17897,#17867);
#17848=PROPERTY_DEFINITION_REPRESENTATION(#17898,#17868);
#17849=PROPERTY_DEFINITION_REPRESENTATION(#17899,#17869);
#17850=PROPERTY_DEFINITION_REPRESENTATION(#17900,#17870);
#17851=PROPERTY_DEFINITION_REPRESENTATION(#17901,#17871);
#17852=PROPERTY_DEFINITION_REPRESENTATION(#17902,#17872);
#17853=PROPERTY_DEFINITION_REPRESENTATION(#17903,#17873);
#17854=PROPERTY_DEFINITION_REPRESENTATION(#17904,#17874);
#17855=PROPERTY_DEFINITION_REPRESENTATION(#17905,#17875);
#17856=PROPERTY_DEFINITION_REPRESENTATION(#17906,#17876);
#17857=PROPERTY_DEFINITION_REPRESENTATION(#17907,#17877);
#17858=PROPERTY_DEFINITION_REPRESENTATION(#17908,#17878);
#17859=PROPERTY_DEFINITION_REPRESENTATION(#17909,#17879);
#17860=PROPERTY_DEFINITION_REPRESENTATION(#17910,#17880);
#17861=PROPERTY_DEFINITION_REPRESENTATION(#17911,#17881);
#17862=PROPERTY_DEFINITION_REPRESENTATION(#17912,#17882);
#17863=PROPERTY_DEFINITION_REPRESENTATION(#17913,#17883);
#17864=PROPERTY_DEFINITION_REPRESENTATION(#17914,#17884);
#17865=REPRESENTATION('material name',(#17885),#36658);
#17866=REPRESENTATION('density',(#17835),#36658);
#17867=REPRESENTATION('material name',(#17886),#36659);
#17868=REPRESENTATION('density',(#17836),#36659);
#17869=REPRESENTATION('material name',(#17887),#36660);
#17870=REPRESENTATION('density',(#17837),#36660);
#17871=REPRESENTATION('material name',(#17888),#36661);
#17872=REPRESENTATION('density',(#17838),#36661);
#17873=REPRESENTATION('material name',(#17889),#36662);
#17874=REPRESENTATION('density',(#17839),#36662);
#17875=REPRESENTATION('material name',(#17890),#36663);
#17876=REPRESENTATION('density',(#17840),#36663);
#17877=REPRESENTATION('material name',(#17891),#36664);
#17878=REPRESENTATION('density',(#17841),#36664);
#17879=REPRESENTATION('material name',(#17892),#36665);
#17880=REPRESENTATION('density',(#17842),#36665);
#17881=REPRESENTATION('material name',(#17893),#36666);
#17882=REPRESENTATION('density',(#17843),#36666);
#17883=REPRESENTATION('material name',(#17894),#36667);
#17884=REPRESENTATION('density',(#17844),#36667);
#17885=DESCRIPTIVE_REPRESENTATION_ITEM('Steel','Steel');
#17886=DESCRIPTIVE_REPRESENTATION_ITEM('Steel','Steel');
#17887=DESCRIPTIVE_REPRESENTATION_ITEM('Steel','Steel');
#17888=DESCRIPTIVE_REPRESENTATION_ITEM('Steel','Steel');
#17889=DESCRIPTIVE_REPRESENTATION_ITEM('Steel','Steel');
#17890=DESCRIPTIVE_REPRESENTATION_ITEM('Steel','Steel');
#17891=DESCRIPTIVE_REPRESENTATION_ITEM('Steel','Steel');
#17892=DESCRIPTIVE_REPRESENTATION_ITEM('Steel','Steel');
#17893=DESCRIPTIVE_REPRESENTATION_ITEM('Steel','Steel');
#17894=DESCRIPTIVE_REPRESENTATION_ITEM('Steel','Steel');
#17895=PROPERTY_DEFINITION('material property','material name',#36718);
#17896=PROPERTY_DEFINITION('material property','density of part',#36718);
#17897=PROPERTY_DEFINITION('material property','material name',#36719);
#17898=PROPERTY_DEFINITION('material property','density of part',#36719);
#17899=PROPERTY_DEFINITION('material property','material name',#36720);
#17900=PROPERTY_DEFINITION('material property','density of part',#36720);
#17901=PROPERTY_DEFINITION('material property','material name',#36721);
#17902=PROPERTY_DEFINITION('material property','density of part',#36721);
#17903=PROPERTY_DEFINITION('material property','material name',#36722);
#17904=PROPERTY_DEFINITION('material property','density of part',#36722);
#17905=PROPERTY_DEFINITION('material property','material name',#36723);
#17906=PROPERTY_DEFINITION('material property','density of part',#36723);
#17907=PROPERTY_DEFINITION('material property','material name',#36724);
#17908=PROPERTY_DEFINITION('material property','density of part',#36724);
#17909=PROPERTY_DEFINITION('material property','material name',#36725);
#17910=PROPERTY_DEFINITION('material property','density of part',#36725);
#17911=PROPERTY_DEFINITION('material property','material name',#36726);
#17912=PROPERTY_DEFINITION('material property','density of part',#36726);
#17913=PROPERTY_DEFINITION('material property','material name',#36727);
#17914=PROPERTY_DEFINITION('material property','density of part',#36727);
#17915=AXIS2_PLACEMENT_3D('',#24194,#19438,#19439);
#17916=AXIS2_PLACEMENT_3D('',#24195,#19440,#19441);
#17917=AXIS2_PLACEMENT_3D('',#24196,#19442,#19443);
#17918=AXIS2_PLACEMENT_3D('',#24206,#19448,#19449);
#17919=AXIS2_PLACEMENT_3D('',#24208,#19450,#19451);
#17920=AXIS2_PLACEMENT_3D('',#24210,#19452,#19453);
#17921=AXIS2_PLACEMENT_3D('',#24212,#19454,#19455);
#17922=AXIS2_PLACEMENT_3D('',#24214,#19456,#19457);
#17923=AXIS2_PLACEMENT_3D('',#24216,#19458,#19459);
#17924=AXIS2_PLACEMENT_3D('',#24218,#19460,#19461);
#17925=AXIS2_PLACEMENT_3D('',#24220,#19462,#19463);
#17926=AXIS2_PLACEMENT_3D('',#24222,#19464,#19465);
#17927=AXIS2_PLACEMENT_3D('',#24224,#19466,#19467);
#17928=AXIS2_PLACEMENT_3D('',#24226,#19468,#19469);
#17929=AXIS2_PLACEMENT_3D('',#24228,#19470,#19471);
#17930=AXIS2_PLACEMENT_3D('',#24230,#19472,#19473);
#17931=AXIS2_PLACEMENT_3D('',#24232,#19474,#19475);
#17932=AXIS2_PLACEMENT_3D('',#24234,#19476,#19477);
#17933=AXIS2_PLACEMENT_3D('',#24236,#19478,#19479);
#17934=AXIS2_PLACEMENT_3D('',#24238,#19480,#19481);
#17935=AXIS2_PLACEMENT_3D('',#24240,#19482,#19483);
#17936=AXIS2_PLACEMENT_3D('',#24242,#19484,#19485);
#17937=AXIS2_PLACEMENT_3D('',#24244,#19486,#19487);
#17938=AXIS2_PLACEMENT_3D('',#24246,#19488,#19489);
#17939=AXIS2_PLACEMENT_3D('',#24248,#19490,#19491);
#17940=AXIS2_PLACEMENT_3D('',#24250,#19492,#19493);
#17941=AXIS2_PLACEMENT_3D('',#24252,#19494,#19495);
#17942=AXIS2_PLACEMENT_3D('',#24254,#19496,#19497);
#17943=AXIS2_PLACEMENT_3D('',#24256,#19498,#19499);
#17944=AXIS2_PLACEMENT_3D('',#24465,#19604,#19605);
#17945=AXIS2_PLACEMENT_3D('',#24683,#19714,#19715);
#17946=AXIS2_PLACEMENT_3D('',#24685,#19716,#19717);
#17947=AXIS2_PLACEMENT_3D('',#24687,#19718,#19719);
#17948=AXIS2_PLACEMENT_3D('',#24689,#19720,#19721);
#17949=AXIS2_PLACEMENT_3D('',#24691,#19722,#19723);
#17950=AXIS2_PLACEMENT_3D('',#24693,#19724,#19725);
#17951=AXIS2_PLACEMENT_3D('',#24695,#19726,#19727);
#17952=AXIS2_PLACEMENT_3D('',#24697,#19728,#19729);
#17953=AXIS2_PLACEMENT_3D('',#24699,#19730,#19731);
#17954=AXIS2_PLACEMENT_3D('',#24701,#19732,#19733);
#17955=AXIS2_PLACEMENT_3D('',#24703,#19734,#19735);
#17956=AXIS2_PLACEMENT_3D('',#24705,#19736,#19737);
#17957=AXIS2_PLACEMENT_3D('',#24707,#19738,#19739);
#17958=AXIS2_PLACEMENT_3D('',#24709,#19740,#19741);
#17959=AXIS2_PLACEMENT_3D('',#24711,#19742,#19743);
#17960=AXIS2_PLACEMENT_3D('',#24713,#19744,#19745);
#17961=AXIS2_PLACEMENT_3D('',#24715,#19746,#19747);
#17962=AXIS2_PLACEMENT_3D('',#24717,#19748,#19749);
#17963=AXIS2_PLACEMENT_3D('',#24719,#19750,#19751);
#17964=AXIS2_PLACEMENT_3D('',#24721,#19752,#19753);
#17965=AXIS2_PLACEMENT_3D('',#24723,#19754,#19755);
#17966=AXIS2_PLACEMENT_3D('',#24725,#19756,#19757);
#17967=AXIS2_PLACEMENT_3D('',#24727,#19758,#19759);
#17968=AXIS2_PLACEMENT_3D('',#24729,#19760,#19761);
#17969=AXIS2_PLACEMENT_3D('',#24731,#19762,#19763);
#17970=AXIS2_PLACEMENT_3D('',#24733,#19764,#19765);
#17971=AXIS2_PLACEMENT_3D('',#24734,#19766,#19767);
#17972=AXIS2_PLACEMENT_3D('',#24737,#19770,#19771);
#17973=AXIS2_PLACEMENT_3D('',#24739,#19773,#19774);
#17974=AXIS2_PLACEMENT_3D('',#24741,#19776,#19777);
#17975=AXIS2_PLACEMENT_3D('',#24743,#19779,#19780);
#17976=AXIS2_PLACEMENT_3D('',#24745,#19782,#19783);
#17977=AXIS2_PLACEMENT_3D('',#24747,#19785,#19786);
#17978=AXIS2_PLACEMENT_3D('',#24749,#19788,#19789);
#17979=AXIS2_PLACEMENT_3D('',#24751,#19791,#19792);
#17980=AXIS2_PLACEMENT_3D('',#24753,#19794,#19795);
#17981=AXIS2_PLACEMENT_3D('',#24755,#19797,#19798);
#17982=AXIS2_PLACEMENT_3D('',#24757,#19800,#19801);
#17983=AXIS2_PLACEMENT_3D('',#24759,#19803,#19804);
#17984=AXIS2_PLACEMENT_3D('',#24761,#19806,#19807);
#17985=AXIS2_PLACEMENT_3D('',#24763,#19809,#19810);
#17986=AXIS2_PLACEMENT_3D('',#24765,#19812,#19813);
#17987=AXIS2_PLACEMENT_3D('',#24767,#19815,#19816);
#17988=AXIS2_PLACEMENT_3D('',#24769,#19818,#19819);
#17989=AXIS2_PLACEMENT_3D('',#24771,#19821,#19822);
#17990=AXIS2_PLACEMENT_3D('',#24773,#19824,#19825);
#17991=AXIS2_PLACEMENT_3D('',#24775,#19827,#19828);
#17992=AXIS2_PLACEMENT_3D('',#24777,#19830,#19831);
#17993=AXIS2_PLACEMENT_3D('',#24779,#19833,#19834);
#17994=AXIS2_PLACEMENT_3D('',#24781,#19836,#19837);
#17995=AXIS2_PLACEMENT_3D('',#24783,#19839,#19840);
#17996=AXIS2_PLACEMENT_3D('',#24785,#19842,#19843);
#17997=AXIS2_PLACEMENT_3D('',#24787,#19845,#19846);
#17998=AXIS2_PLACEMENT_3D('',#24789,#19848,#19849);
#17999=AXIS2_PLACEMENT_3D('',#24792,#19852,#19853);
#18000=AXIS2_PLACEMENT_3D('',#24795,#19856,#19857);
#18001=AXIS2_PLACEMENT_3D('',#24798,#19860,#19861);
#18002=AXIS2_PLACEMENT_3D('',#24801,#19864,#19865);
#18003=AXIS2_PLACEMENT_3D('',#24804,#19868,#19869);
#18004=AXIS2_PLACEMENT_3D('',#24807,#19872,#19873);
#18005=AXIS2_PLACEMENT_3D('',#24810,#19876,#19877);
#18006=AXIS2_PLACEMENT_3D('',#24813,#19880,#19881);
#18007=AXIS2_PLACEMENT_3D('',#24816,#19884,#19885);
#18008=AXIS2_PLACEMENT_3D('',#24819,#19888,#19889);
#18009=AXIS2_PLACEMENT_3D('',#24822,#19892,#19893);
#18010=AXIS2_PLACEMENT_3D('',#24825,#19896,#19897);
#18011=AXIS2_PLACEMENT_3D('',#24828,#19900,#19901);
#18012=AXIS2_PLACEMENT_3D('',#24831,#19904,#19905);
#18013=AXIS2_PLACEMENT_3D('',#24834,#19908,#19909);
#18014=AXIS2_PLACEMENT_3D('',#24837,#19912,#19913);
#18015=AXIS2_PLACEMENT_3D('',#24840,#19916,#19917);
#18016=AXIS2_PLACEMENT_3D('',#24843,#19920,#19921);
#18017=AXIS2_PLACEMENT_3D('',#24846,#19924,#19925);
#18018=AXIS2_PLACEMENT_3D('',#24849,#19928,#19929);
#18019=AXIS2_PLACEMENT_3D('',#24852,#19932,#19933);
#18020=AXIS2_PLACEMENT_3D('',#24855,#19936,#19937);
#18021=AXIS2_PLACEMENT_3D('',#24858,#19940,#19941);
#18022=AXIS2_PLACEMENT_3D('',#24861,#19944,#19945);
#18023=AXIS2_PLACEMENT_3D('',#24864,#19948,#19949);
#18024=AXIS2_PLACEMENT_3D('',#24867,#19952,#19953);
#18025=AXIS2_PLACEMENT_3D('',#24869,#19955,#19956);
#18026=AXIS2_PLACEMENT_3D('',#24871,#19958,#19959);
#18027=AXIS2_PLACEMENT_3D('',#24873,#19961,#19962);
#18028=AXIS2_PLACEMENT_3D('',#24875,#19964,#19965);
#18029=AXIS2_PLACEMENT_3D('',#24876,#19966,#19967);
#18030=AXIS2_PLACEMENT_3D('',#24878,#19969,#19970);
#18031=AXIS2_PLACEMENT_3D('',#24880,#19972,#19973);
#18032=AXIS2_PLACEMENT_3D('',#24881,#19974,#19975);
#18033=AXIS2_PLACEMENT_3D('',#24883,#19977,#19978);
#18034=AXIS2_PLACEMENT_3D('',#24885,#19980,#19981);
#18035=AXIS2_PLACEMENT_3D('',#24886,#19982,#19983);
#18036=AXIS2_PLACEMENT_3D('',#24888,#19985,#19986);
#18037=AXIS2_PLACEMENT_3D('',#24890,#19988,#19989);
#18038=AXIS2_PLACEMENT_3D('',#24891,#19990,#19991);
#18039=AXIS2_PLACEMENT_3D('',#24893,#19993,#19994);
#18040=AXIS2_PLACEMENT_3D('',#24895,#19996,#19997);
#18041=AXIS2_PLACEMENT_3D('',#24896,#19998,#19999);
#18042=AXIS2_PLACEMENT_3D('',#24898,#20001,#20002);
#18043=AXIS2_PLACEMENT_3D('',#24900,#20004,#20005);
#18044=AXIS2_PLACEMENT_3D('',#24901,#20006,#20007);
#18045=AXIS2_PLACEMENT_3D('',#24903,#20009,#20010);
#18046=AXIS2_PLACEMENT_3D('',#24905,#20012,#20013);
#18047=AXIS2_PLACEMENT_3D('',#24906,#20014,#20015);
#18048=AXIS2_PLACEMENT_3D('',#24908,#20017,#20018);
#18049=AXIS2_PLACEMENT_3D('',#24910,#20020,#20021);
#18050=AXIS2_PLACEMENT_3D('',#24911,#20022,#20023);
#18051=AXIS2_PLACEMENT_3D('',#24913,#20025,#20026);
#18052=AXIS2_PLACEMENT_3D('',#24915,#20028,#20029);
#18053=AXIS2_PLACEMENT_3D('',#24916,#20030,#20031);
#18054=AXIS2_PLACEMENT_3D('',#24918,#20033,#20034);
#18055=AXIS2_PLACEMENT_3D('',#24920,#20036,#20037);
#18056=AXIS2_PLACEMENT_3D('',#24921,#20038,#20039);
#18057=AXIS2_PLACEMENT_3D('',#24923,#20041,#20042);
#18058=AXIS2_PLACEMENT_3D('',#24925,#20044,#20045);
#18059=AXIS2_PLACEMENT_3D('',#24926,#20046,#20047);
#18060=AXIS2_PLACEMENT_3D('',#24928,#20049,#20050);
#18061=AXIS2_PLACEMENT_3D('',#24930,#20052,#20053);
#18062=AXIS2_PLACEMENT_3D('',#24931,#20054,#20055);
#18063=AXIS2_PLACEMENT_3D('',#24933,#20057,#20058);
#18064=AXIS2_PLACEMENT_3D('',#24935,#20060,#20061);
#18065=AXIS2_PLACEMENT_3D('',#24936,#20062,#20063);
#18066=AXIS2_PLACEMENT_3D('',#24938,#20065,#20066);
#18067=AXIS2_PLACEMENT_3D('',#24940,#20068,#20069);
#18068=AXIS2_PLACEMENT_3D('',#24941,#20070,#20071);
#18069=AXIS2_PLACEMENT_3D('',#24943,#20073,#20074);
#18070=AXIS2_PLACEMENT_3D('',#24945,#20076,#20077);
#18071=AXIS2_PLACEMENT_3D('',#24946,#20078,#20079);
#18072=AXIS2_PLACEMENT_3D('',#24948,#20081,#20082);
#18073=AXIS2_PLACEMENT_3D('',#24950,#20084,#20085);
#18074=AXIS2_PLACEMENT_3D('',#24951,#20086,#20087);
#18075=AXIS2_PLACEMENT_3D('',#24953,#20089,#20090);
#18076=AXIS2_PLACEMENT_3D('',#24955,#20092,#20093);
#18077=AXIS2_PLACEMENT_3D('',#24956,#20094,#20095);
#18078=AXIS2_PLACEMENT_3D('',#24958,#20097,#20098);
#18079=AXIS2_PLACEMENT_3D('',#24960,#20100,#20101);
#18080=AXIS2_PLACEMENT_3D('',#24961,#20102,#20103);
#18081=AXIS2_PLACEMENT_3D('',#24963,#20105,#20106);
#18082=AXIS2_PLACEMENT_3D('',#24965,#20108,#20109);
#18083=AXIS2_PLACEMENT_3D('',#24966,#20110,#20111);
#18084=AXIS2_PLACEMENT_3D('',#24968,#20113,#20114);
#18085=AXIS2_PLACEMENT_3D('',#24970,#20116,#20117);
#18086=AXIS2_PLACEMENT_3D('',#24971,#20118,#20119);
#18087=AXIS2_PLACEMENT_3D('',#24973,#20121,#20122);
#18088=AXIS2_PLACEMENT_3D('',#24975,#20124,#20125);
#18089=AXIS2_PLACEMENT_3D('',#24976,#20126,#20127);
#18090=AXIS2_PLACEMENT_3D('',#24978,#20129,#20130);
#18091=AXIS2_PLACEMENT_3D('',#24980,#20132,#20133);
#18092=AXIS2_PLACEMENT_3D('',#24981,#20134,#20135);
#18093=AXIS2_PLACEMENT_3D('',#24983,#20137,#20138);
#18094=AXIS2_PLACEMENT_3D('',#24985,#20140,#20141);
#18095=AXIS2_PLACEMENT_3D('',#24986,#20142,#20143);
#18096=AXIS2_PLACEMENT_3D('',#24988,#20145,#20146);
#18097=AXIS2_PLACEMENT_3D('',#24990,#20148,#20149);
#18098=AXIS2_PLACEMENT_3D('',#24991,#20150,#20151);
#18099=AXIS2_PLACEMENT_3D('',#24993,#20153,#20154);
#18100=AXIS2_PLACEMENT_3D('',#24995,#20156,#20157);
#18101=AXIS2_PLACEMENT_3D('',#24996,#20158,#20159);
#18102=AXIS2_PLACEMENT_3D('',#24998,#20161,#20162);
#18103=AXIS2_PLACEMENT_3D('',#25000,#20164,#20165);
#18104=AXIS2_PLACEMENT_3D('',#25001,#20166,#20167);
#18105=AXIS2_PLACEMENT_3D('',#25002,#20168,#20169);
#18106=AXIS2_PLACEMENT_3D('',#25003,#20170,#20171);
#18107=AXIS2_PLACEMENT_3D('',#25006,#20172,#20173);
#18108=AXIS2_PLACEMENT_3D('',#25008,#20174,#20175);
#18109=AXIS2_PLACEMENT_3D('',#25012,#20177,#20178);
#18110=AXIS2_PLACEMENT_3D('',#25014,#20179,#20180);
#18111=AXIS2_PLACEMENT_3D('',#25016,#20182,#20183);
#18112=AXIS2_PLACEMENT_3D('',#25018,#20185,#20186);
#18113=AXIS2_PLACEMENT_3D('',#25020,#20188,#20189);
#18114=AXIS2_PLACEMENT_3D('',#25023,#20190,#20191);
#18115=AXIS2_PLACEMENT_3D('',#25025,#20192,#20193);
#18116=AXIS2_PLACEMENT_3D('',#25029,#20195,#20196);
#18117=AXIS2_PLACEMENT_3D('',#25031,#20197,#20198);
#18118=AXIS2_PLACEMENT_3D('',#25033,#20200,#20201);
#18119=AXIS2_PLACEMENT_3D('',#25035,#20203,#20204);
#18120=AXIS2_PLACEMENT_3D('',#25037,#20206,#20207);
#18121=AXIS2_PLACEMENT_3D('',#25040,#20208,#20209);
#18122=AXIS2_PLACEMENT_3D('',#25042,#20210,#20211);
#18123=AXIS2_PLACEMENT_3D('',#25046,#20213,#20214);
#18124=AXIS2_PLACEMENT_3D('',#25048,#20215,#20216);
#18125=AXIS2_PLACEMENT_3D('',#25050,#20218,#20219);
#18126=AXIS2_PLACEMENT_3D('',#25052,#20221,#20222);
#18127=AXIS2_PLACEMENT_3D('',#25065,#20224,#20225);
#18128=AXIS2_PLACEMENT_3D('',#25067,#20226,#20227);
#18129=AXIS2_PLACEMENT_3D('',#25069,#20228,#20229);
#18130=AXIS2_PLACEMENT_3D('',#25070,#20230,#20231);
#18131=AXIS2_PLACEMENT_3D('',#25071,#20232,#20233);
#18132=AXIS2_PLACEMENT_3D('',#25074,#20234,#20235);
#18133=AXIS2_PLACEMENT_3D('',#25077,#20237,#20238);
#18134=AXIS2_PLACEMENT_3D('',#25079,#20240,#20241);
#18135=AXIS2_PLACEMENT_3D('',#25080,#20242,#20243);
#18136=AXIS2_PLACEMENT_3D('',#25081,#20244,#20245);
#18137=AXIS2_PLACEMENT_3D('',#25084,#20246,#20247);
#18138=AXIS2_PLACEMENT_3D('',#25095,#20254,#20255);
#18139=AXIS2_PLACEMENT_3D('',#25096,#20256,#20257);
#18140=AXIS2_PLACEMENT_3D('',#25097,#20258,#20259);
#18141=AXIS2_PLACEMENT_3D('',#25100,#20260,#20261);
#18142=AXIS2_PLACEMENT_3D('',#25102,#20262,#20263);
#18143=AXIS2_PLACEMENT_3D('',#25116,#20266,#20267);
#18144=AXIS2_PLACEMENT_3D('',#25118,#20268,#20269);
#18145=AXIS2_PLACEMENT_3D('',#25119,#20270,#20271);
#18146=AXIS2_PLACEMENT_3D('',#25120,#20272,#20273);
#18147=AXIS2_PLACEMENT_3D('',#25121,#20274,#20275);
#18148=AXIS2_PLACEMENT_3D('',#25126,#20278,#20279);
#18149=AXIS2_PLACEMENT_3D('',#25127,#20280,#20281);
#18150=AXIS2_PLACEMENT_3D('',#25132,#20283,#20284);
#18151=AXIS2_PLACEMENT_3D('',#25138,#20288,#20289);
#18152=AXIS2_PLACEMENT_3D('',#25144,#20293,#20294);
#18153=AXIS2_PLACEMENT_3D('',#25150,#20298,#20299);
#18154=AXIS2_PLACEMENT_3D('',#25156,#20303,#20304);
#18155=AXIS2_PLACEMENT_3D('',#25163,#20308,#20309);
#18156=AXIS2_PLACEMENT_3D('',#25164,#20310,#20311);
#18157=AXIS2_PLACEMENT_3D('',#25167,#20314,#20315);
#18158=AXIS2_PLACEMENT_3D('',#25170,#20316,#20317);
#18159=AXIS2_PLACEMENT_3D('',#25174,#20319,#20320);
#18160=AXIS2_PLACEMENT_3D('',#25176,#20322,#20323);
#18161=AXIS2_PLACEMENT_3D('',#25182,#20326,#20327);
#18162=AXIS2_PLACEMENT_3D('',#25185,#20329,#20330);
#18163=AXIS2_PLACEMENT_3D('',#25186,#20331,#20332);
#18164=AXIS2_PLACEMENT_3D('',#25194,#20338,#20339);
#18165=AXIS2_PLACEMENT_3D('',#25196,#20341,#20342);
#18166=AXIS2_PLACEMENT_3D('',#25203,#20347,#20348);
#18167=AXIS2_PLACEMENT_3D('',#25204,#20349,#20350);
#18168=AXIS2_PLACEMENT_3D('',#25207,#20351,#20352);
#18169=AXIS2_PLACEMENT_3D('',#25211,#20354,#20355);
#18170=AXIS2_PLACEMENT_3D('',#25213,#20357,#20358);
#18171=AXIS2_PLACEMENT_3D('',#25216,#20359,#20360);
#18172=AXIS2_PLACEMENT_3D('',#25220,#20362,#20363);
#18173=AXIS2_PLACEMENT_3D('',#25222,#20365,#20366);
#18174=AXIS2_PLACEMENT_3D('',#25225,#20367,#20368);
#18175=AXIS2_PLACEMENT_3D('',#25229,#20370,#20371);
#18176=AXIS2_PLACEMENT_3D('',#25231,#20373,#20374);
#18177=AXIS2_PLACEMENT_3D('',#25234,#20375,#20376);
#18178=AXIS2_PLACEMENT_3D('',#25238,#20378,#20379);
#18179=AXIS2_PLACEMENT_3D('',#25240,#20381,#20382);
#18180=AXIS2_PLACEMENT_3D('',#25249,#20387,#20388);
#18181=AXIS2_PLACEMENT_3D('',#25255,#20392,#20393);
#18182=AXIS2_PLACEMENT_3D('',#25261,#20397,#20398);
#18183=AXIS2_PLACEMENT_3D('',#25267,#20402,#20403);
#18184=AXIS2_PLACEMENT_3D('',#25273,#20407,#20408);
#18185=AXIS2_PLACEMENT_3D('',#25279,#20412,#20413);
#18186=AXIS2_PLACEMENT_3D('',#25285,#20417,#20418);
#18187=AXIS2_PLACEMENT_3D('',#25294,#20423,#20424);
#18188=AXIS2_PLACEMENT_3D('',#25303,#20429,#20430);
#18189=AXIS2_PLACEMENT_3D('',#25308,#20434,#20435);
#18190=AXIS2_PLACEMENT_3D('',#25314,#20439,#20440);
#18191=AXIS2_PLACEMENT_3D('',#25317,#20443,#20444);
#18192=AXIS2_PLACEMENT_3D('',#25320,#20447,#20448);
#18193=AXIS2_PLACEMENT_3D('',#25326,#20452,#20453);
#18194=AXIS2_PLACEMENT_3D('',#25331,#20457,#20458);
#18195=AXIS2_PLACEMENT_3D('',#25333,#20460,#20461);
#18196=AXIS2_PLACEMENT_3D('',#25337,#20464,#20465);
#18197=AXIS2_PLACEMENT_3D('',#25342,#20469,#20470);
#18198=AXIS2_PLACEMENT_3D('',#25345,#20471,#20472);
#18199=AXIS2_PLACEMENT_3D('',#25349,#20474,#20475);
#18200=AXIS2_PLACEMENT_3D('',#25351,#20477,#20478);
#18201=AXIS2_PLACEMENT_3D('',#25354,#20479,#20480);
#18202=AXIS2_PLACEMENT_3D('',#25358,#20482,#20483);
#18203=AXIS2_PLACEMENT_3D('',#25360,#20485,#20486);
#18204=AXIS2_PLACEMENT_3D('',#25362,#20487,#20488);
#18205=AXIS2_PLACEMENT_3D('',#25365,#20490,#20491);
#18206=AXIS2_PLACEMENT_3D('',#25367,#20493,#20494);
#18207=AXIS2_PLACEMENT_3D('',#25369,#20495,#20496);
#18208=AXIS2_PLACEMENT_3D('',#25372,#20498,#20499);
#18209=AXIS2_PLACEMENT_3D('',#25374,#20501,#20502);
#18210=AXIS2_PLACEMENT_3D('',#25379,#20507,#20508);
#18211=AXIS2_PLACEMENT_3D('',#25382,#20511,#20512);
#18212=AXIS2_PLACEMENT_3D('',#25383,#20513,#20514);
#18213=AXIS2_PLACEMENT_3D('',#25386,#20517,#20518);
#18214=AXIS2_PLACEMENT_3D('',#25388,#20520,#20521);
#18215=AXIS2_PLACEMENT_3D('',#25389,#20522,#20523);
#18216=AXIS2_PLACEMENT_3D('',#25393,#20526,#20527);
#18217=AXIS2_PLACEMENT_3D('',#25397,#20530,#20531);
#18218=AXIS2_PLACEMENT_3D('',#25406,#20536,#20537);
#18219=AXIS2_PLACEMENT_3D('',#25408,#20538,#20539);
#18220=AXIS2_PLACEMENT_3D('',#25412,#20542,#20543);
#18221=AXIS2_PLACEMENT_3D('',#25413,#20544,#20545);
#18222=AXIS2_PLACEMENT_3D('',#25414,#20546,#20547);
#18223=AXIS2_PLACEMENT_3D('',#25418,#20550,#20551);
#18224=AXIS2_PLACEMENT_3D('',#25419,#20552,#20553);
#18225=AXIS2_PLACEMENT_3D('',#25428,#20558,#20559);
#18226=AXIS2_PLACEMENT_3D('',#25430,#20560,#20561);
#18227=AXIS2_PLACEMENT_3D('',#25434,#20564,#20565);
#18228=AXIS2_PLACEMENT_3D('',#25435,#20566,#20567);
#18229=AXIS2_PLACEMENT_3D('',#25440,#20570,#20571);
#18230=AXIS2_PLACEMENT_3D('',#25441,#20572,#20573);
#18231=AXIS2_PLACEMENT_3D('',#25442,#20574,#20575);
#18232=AXIS2_PLACEMENT_3D('',#25447,#20577,#20578);
#18233=AXIS2_PLACEMENT_3D('',#25450,#20580,#20581);
#18234=AXIS2_PLACEMENT_3D('',#25451,#20582,#20583);
#18235=AXIS2_PLACEMENT_3D('',#25457,#20587,#20588);
#18236=AXIS2_PLACEMENT_3D('',#25461,#20590,#20591);
#18237=AXIS2_PLACEMENT_3D('',#25462,#20592,#20593);
#18238=AXIS2_PLACEMENT_3D('',#25463,#20594,#20595);
#18239=AXIS2_PLACEMENT_3D('',#25466,#20598,#20599);
#18240=AXIS2_PLACEMENT_3D('',#25471,#20601,#20602);
#18241=AXIS2_PLACEMENT_3D('',#25474,#20604,#20605);
#18242=AXIS2_PLACEMENT_3D('',#25475,#20606,#20607);
#18243=AXIS2_PLACEMENT_3D('',#25481,#20611,#20612);
#18244=AXIS2_PLACEMENT_3D('',#25485,#20614,#20615);
#18245=AXIS2_PLACEMENT_3D('',#25486,#20616,#20617);
#18246=AXIS2_PLACEMENT_3D('',#25487,#20618,#20619);
#18247=AXIS2_PLACEMENT_3D('',#25490,#20622,#20623);
#18248=AXIS2_PLACEMENT_3D('',#25493,#20624,#20625);
#18249=AXIS2_PLACEMENT_3D('',#25501,#20630,#20631);
#18250=AXIS2_PLACEMENT_3D('',#25506,#20635,#20636);
#18251=AXIS2_PLACEMENT_3D('',#25509,#20638,#20639);
#18252=AXIS2_PLACEMENT_3D('',#25510,#20640,#20641);
#18253=AXIS2_PLACEMENT_3D('',#25516,#20645,#20646);
#18254=AXIS2_PLACEMENT_3D('',#25519,#20649,#20650);
#18255=AXIS2_PLACEMENT_3D('',#25520,#20651,#20652);
#18256=AXIS2_PLACEMENT_3D('',#25526,#20657,#20658);
#18257=AXIS2_PLACEMENT_3D('',#25530,#20661,#20662);
#18258=AXIS2_PLACEMENT_3D('',#25538,#20670,#20671);
#18259=AXIS2_PLACEMENT_3D('',#25540,#20673,#20674);
#18260=AXIS2_PLACEMENT_3D('',#25547,#20679,#20680);
#18261=AXIS2_PLACEMENT_3D('',#25549,#20682,#20683);
#18262=AXIS2_PLACEMENT_3D('',#25550,#20684,#20685);
#18263=AXIS2_PLACEMENT_3D('',#25551,#20686,#20687);
#18264=AXIS2_PLACEMENT_3D('',#25552,#20688,#20689);
#18265=AXIS2_PLACEMENT_3D('',#25553,#20690,#20691);
#18266=AXIS2_PLACEMENT_3D('',#25554,#20692,#20693);
#18267=AXIS2_PLACEMENT_3D('',#25555,#20694,#20695);
#18268=AXIS2_PLACEMENT_3D('',#25556,#20696,#20697);
#18269=AXIS2_PLACEMENT_3D('',#25557,#20698,#20699);
#18270=AXIS2_PLACEMENT_3D('',#25558,#20700,#20701);
#18271=AXIS2_PLACEMENT_3D('',#25559,#20702,#20703);
#18272=AXIS2_PLACEMENT_3D('',#25562,#20704,#20705);
#18273=AXIS2_PLACEMENT_3D('',#25564,#20706,#20707);
#18274=AXIS2_PLACEMENT_3D('',#25565,#20708,#20709);
#18275=AXIS2_PLACEMENT_3D('',#25566,#20710,#20711);
#18276=AXIS2_PLACEMENT_3D('',#25569,#20712,#20713);
#18277=AXIS2_PLACEMENT_3D('',#25571,#20714,#20715);
#18278=AXIS2_PLACEMENT_3D('',#25572,#20716,#20717);
#18279=AXIS2_PLACEMENT_3D('',#25573,#20718,#20719);
#18280=AXIS2_PLACEMENT_3D('',#25576,#20720,#20721);
#18281=AXIS2_PLACEMENT_3D('',#25578,#20722,#20723);
#18282=AXIS2_PLACEMENT_3D('',#25580,#20724,#20725);
#18283=AXIS2_PLACEMENT_3D('',#25593,#20726,#20727);
#18284=AXIS2_PLACEMENT_3D('',#25596,#20728,#20729);
#18285=AXIS2_PLACEMENT_3D('',#25598,#20730,#20731);
#18286=AXIS2_PLACEMENT_3D('',#25599,#20732,#20733);
#18287=AXIS2_PLACEMENT_3D('',#25600,#20734,#20735);
#18288=AXIS2_PLACEMENT_3D('',#25603,#20736,#20737);
#18289=AXIS2_PLACEMENT_3D('',#25605,#20738,#20739);
#18290=AXIS2_PLACEMENT_3D('',#25607,#20740,#20741);
#18291=AXIS2_PLACEMENT_3D('',#25620,#20742,#20743);
#18292=AXIS2_PLACEMENT_3D('',#25623,#20744,#20745);
#18293=AXIS2_PLACEMENT_3D('',#25625,#20746,#20747);
#18294=AXIS2_PLACEMENT_3D('',#25626,#20748,#20749);
#18295=AXIS2_PLACEMENT_3D('',#25627,#20750,#20751);
#18296=AXIS2_PLACEMENT_3D('',#25630,#20752,#20753);
#18297=AXIS2_PLACEMENT_3D('',#25632,#20754,#20755);
#18298=AXIS2_PLACEMENT_3D('',#25646,#20756,#20757);
#18299=AXIS2_PLACEMENT_3D('',#25647,#20758,#20759);
#18300=AXIS2_PLACEMENT_3D('',#25650,#20760,#20761);
#18301=AXIS2_PLACEMENT_3D('',#25665,#20762,#20763);
#18302=AXIS2_PLACEMENT_3D('',#25666,#20764,#20765);
#18303=AXIS2_PLACEMENT_3D('',#25667,#20766,#20767);
#18304=AXIS2_PLACEMENT_3D('',#25670,#20768,#20769);
#18305=AXIS2_PLACEMENT_3D('',#25672,#20770,#20771);
#18306=AXIS2_PLACEMENT_3D('',#25673,#20772,#20773);
#18307=AXIS2_PLACEMENT_3D('',#25674,#20774,#20775);
#18308=AXIS2_PLACEMENT_3D('',#25677,#20776,#20777);
#18309=AXIS2_PLACEMENT_3D('',#25679,#20778,#20779);
#18310=AXIS2_PLACEMENT_3D('',#25680,#20780,#20781);
#18311=AXIS2_PLACEMENT_3D('',#25681,#20782,#20783);
#18312=AXIS2_PLACEMENT_3D('',#25683,#20784,#20785);
#18313=AXIS2_PLACEMENT_3D('',#25685,#20786,#20787);
#18314=AXIS2_PLACEMENT_3D('',#25686,#20788,#20789);
#18315=AXIS2_PLACEMENT_3D('',#25687,#20790,#20791);
#18316=AXIS2_PLACEMENT_3D('',#25690,#20792,#20793);
#18317=AXIS2_PLACEMENT_3D('',#25691,#20794,#20795);
#18318=AXIS2_PLACEMENT_3D('',#25693,#20796,#20797);
#18319=AXIS2_PLACEMENT_3D('',#25694,#20798,#20799);
#18320=AXIS2_PLACEMENT_3D('',#25695,#20800,#20801);
#18321=AXIS2_PLACEMENT_3D('',#25697,#20802,#20803);
#18322=AXIS2_PLACEMENT_3D('',#25699,#20804,#20805);
#18323=AXIS2_PLACEMENT_3D('',#25701,#20806,#20807);
#18324=AXIS2_PLACEMENT_3D('',#25702,#20808,#20809);
#18325=AXIS2_PLACEMENT_3D('',#25703,#20810,#20811);
#18326=AXIS2_PLACEMENT_3D('',#25705,#20812,#20813);
#18327=AXIS2_PLACEMENT_3D('',#25707,#20814,#20815);
#18328=AXIS2_PLACEMENT_3D('',#25708,#20816,#20817);
#18329=AXIS2_PLACEMENT_3D('',#25709,#20818,#20819);
#18330=AXIS2_PLACEMENT_3D('',#25711,#20820,#20821);
#18331=AXIS2_PLACEMENT_3D('',#25713,#20822,#20823);
#18332=AXIS2_PLACEMENT_3D('',#25715,#20824,#20825);
#18333=AXIS2_PLACEMENT_3D('',#25716,#20826,#20827);
#18334=AXIS2_PLACEMENT_3D('',#25717,#20828,#20829);
#18335=AXIS2_PLACEMENT_3D('',#25719,#20830,#20831);
#18336=AXIS2_PLACEMENT_3D('',#25721,#20832,#20833);
#18337=AXIS2_PLACEMENT_3D('',#25722,#20834,#20835);
#18338=AXIS2_PLACEMENT_3D('',#25723,#20836,#20837);
#18339=AXIS2_PLACEMENT_3D('',#25725,#20838,#20839);
#18340=AXIS2_PLACEMENT_3D('',#25727,#20840,#20841);
#18341=AXIS2_PLACEMENT_3D('',#25728,#20842,#20843);
#18342=AXIS2_PLACEMENT_3D('',#25729,#20844,#20845);
#18343=AXIS2_PLACEMENT_3D('',#25731,#20846,#20847);
#18344=AXIS2_PLACEMENT_3D('',#25733,#20848,#20849);
#18345=AXIS2_PLACEMENT_3D('',#25734,#20850,#20851);
#18346=AXIS2_PLACEMENT_3D('',#25735,#20852,#20853);
#18347=AXIS2_PLACEMENT_3D('',#25737,#20854,#20855);
#18348=AXIS2_PLACEMENT_3D('',#25739,#20856,#20857);
#18349=AXIS2_PLACEMENT_3D('',#25740,#20858,#20859);
#18350=AXIS2_PLACEMENT_3D('',#25741,#20860,#20861);
#18351=AXIS2_PLACEMENT_3D('',#25743,#20863,#20864);
#18352=AXIS2_PLACEMENT_3D('',#25747,#20866,#20867);
#18353=AXIS2_PLACEMENT_3D('',#25769,#20868,#20869);
#18354=AXIS2_PLACEMENT_3D('',#25776,#20870,#20871);
#18355=AXIS2_PLACEMENT_3D('',#25785,#20872,#20873);
#18356=AXIS2_PLACEMENT_3D('',#25807,#20874,#20875);
#18357=AXIS2_PLACEMENT_3D('',#25829,#20876,#20877);
#18358=AXIS2_PLACEMENT_3D('',#25837,#20878,#20879);
#18359=AXIS2_PLACEMENT_3D('',#25859,#20880,#20881);
#18360=AXIS2_PLACEMENT_3D('',#25880,#20882,#20883);
#18361=AXIS2_PLACEMENT_3D('',#25889,#20884,#20885);
#18362=AXIS2_PLACEMENT_3D('',#25910,#20886,#20887);
#18363=AXIS2_PLACEMENT_3D('',#25911,#20888,#20889);
#18364=AXIS2_PLACEMENT_3D('',#25914,#20890,#20891);
#18365=AXIS2_PLACEMENT_3D('',#25961,#20892,#20893);
#18366=AXIS2_PLACEMENT_3D('',#26008,#20894,#20895);
#18367=AXIS2_PLACEMENT_3D('',#26010,#20896,#20897);
#18368=AXIS2_PLACEMENT_3D('',#26013,#20899,#20900);
#18369=AXIS2_PLACEMENT_3D('',#26060,#20901,#20902);
#18370=AXIS2_PLACEMENT_3D('',#26107,#20903,#20904);
#18371=AXIS2_PLACEMENT_3D('',#26152,#20905,#20906);
#18372=AXIS2_PLACEMENT_3D('',#26153,#20907,#20908);
#18373=AXIS2_PLACEMENT_3D('',#26155,#20910,#20911);
#18374=AXIS2_PLACEMENT_3D('',#26156,#20912,#20913);
#18375=AXIS2_PLACEMENT_3D('',#26158,#20915,#20916);
#18376=AXIS2_PLACEMENT_3D('',#26160,#20917,#20918);
#18377=AXIS2_PLACEMENT_3D('',#26161,#20919,#20920);
#18378=AXIS2_PLACEMENT_3D('',#26163,#20922,#20923);
#18379=AXIS2_PLACEMENT_3D('',#26165,#20925,#20926);
#18380=AXIS2_PLACEMENT_3D('',#26166,#20927,#20928);
#18381=AXIS2_PLACEMENT_3D('',#26169,#20929,#20930);
#18382=AXIS2_PLACEMENT_3D('',#26170,#20931,#20932);
#18383=AXIS2_PLACEMENT_3D('',#26172,#20933,#20934);
#18384=AXIS2_PLACEMENT_3D('',#26173,#20935,#20936);
#18385=AXIS2_PLACEMENT_3D('',#26174,#20937,#20938);
#18386=AXIS2_PLACEMENT_3D('',#26176,#20939,#20940);
#18387=AXIS2_PLACEMENT_3D('',#26178,#20941,#20942);
#18388=AXIS2_PLACEMENT_3D('',#26179,#20943,#20944);
#18389=AXIS2_PLACEMENT_3D('',#26180,#20945,#20946);
#18390=AXIS2_PLACEMENT_3D('',#26183,#20947,#20948);
#18391=AXIS2_PLACEMENT_3D('',#26184,#20949,#20950);
#18392=AXIS2_PLACEMENT_3D('',#26186,#20951,#20952);
#18393=AXIS2_PLACEMENT_3D('',#26187,#20953,#20954);
#18394=AXIS2_PLACEMENT_3D('',#26188,#20955,#20956);
#18395=AXIS2_PLACEMENT_3D('',#26192,#20958,#20959);
#18396=AXIS2_PLACEMENT_3D('',#26194,#20961,#20962);
#18397=AXIS2_PLACEMENT_3D('',#26195,#20963,#20964);
#18398=AXIS2_PLACEMENT_3D('',#26196,#20965,#20966);
#18399=AXIS2_PLACEMENT_3D('',#26197,#20967,#20968);
#18400=AXIS2_PLACEMENT_3D('',#26199,#20969,#20970);
#18401=AXIS2_PLACEMENT_3D('',#26200,#20971,#20972);
#18402=AXIS2_PLACEMENT_3D('',#26201,#20973,#20974);
#18403=AXIS2_PLACEMENT_3D('',#26222,#20978,#20979);
#18404=AXIS2_PLACEMENT_3D('',#26244,#20982,#20983);
#18405=AXIS2_PLACEMENT_3D('',#26245,#20984,#20985);
#18406=AXIS2_PLACEMENT_3D('',#26246,#20986,#20987);
#18407=AXIS2_PLACEMENT_3D('',#26247,#20988,#20989);
#18408=AXIS2_PLACEMENT_3D('',#26248,#20990,#20991);
#18409=AXIS2_PLACEMENT_3D('',#26250,#20992,#20993);
#18410=AXIS2_PLACEMENT_3D('',#26251,#20994,#20995);
#18411=AXIS2_PLACEMENT_3D('',#26252,#20996,#20997);
#18412=AXIS2_PLACEMENT_3D('',#26271,#20998,#20999);
#18413=AXIS2_PLACEMENT_3D('',#26272,#21000,#21001);
#18414=AXIS2_PLACEMENT_3D('',#26273,#21002,#21003);
#18415=AXIS2_PLACEMENT_3D('',#26292,#21004,#21005);
#18416=AXIS2_PLACEMENT_3D('',#26293,#21006,#21007);
#18417=AXIS2_PLACEMENT_3D('',#26294,#21008,#21009);
#18418=AXIS2_PLACEMENT_3D('',#26297,#21012,#21013);
#18419=AXIS2_PLACEMENT_3D('',#26320,#21017,#21018);
#18420=AXIS2_PLACEMENT_3D('',#26325,#21022,#21023);
#18421=AXIS2_PLACEMENT_3D('',#26328,#21024,#21025);
#18422=AXIS2_PLACEMENT_3D('',#26331,#21027,#21028);
#18423=AXIS2_PLACEMENT_3D('',#26333,#21030,#21031);
#18424=AXIS2_PLACEMENT_3D('',#26336,#21032,#21033);
#18425=AXIS2_PLACEMENT_3D('',#26356,#21036,#21037);
#18426=AXIS2_PLACEMENT_3D('',#26373,#21038,#21039);
#18427=AXIS2_PLACEMENT_3D('',#26374,#21040,#21041);
#18428=AXIS2_PLACEMENT_3D('',#26375,#21042,#21043);
#18429=AXIS2_PLACEMENT_3D('',#26377,#21044,#21045);
#18430=AXIS2_PLACEMENT_3D('',#26378,#21046,#21047);
#18431=AXIS2_PLACEMENT_3D('',#26379,#21048,#21049);
#18432=AXIS2_PLACEMENT_3D('',#26381,#21050,#21051);
#18433=AXIS2_PLACEMENT_3D('',#26383,#21052,#21053);
#18434=AXIS2_PLACEMENT_3D('',#26400,#21054,#21055);
#18435=AXIS2_PLACEMENT_3D('',#26405,#21059,#21060);
#18436=AXIS2_PLACEMENT_3D('',#26407,#21061,#21062);
#18437=AXIS2_PLACEMENT_3D('',#26408,#21063,#21064);
#18438=AXIS2_PLACEMENT_3D('',#26409,#21065,#21066);
#18439=AXIS2_PLACEMENT_3D('',#26412,#21069,#21070);
#18440=AXIS2_PLACEMENT_3D('',#26413,#21071,#21072);
#18441=AXIS2_PLACEMENT_3D('',#26414,#21073,#21074);
#18442=AXIS2_PLACEMENT_3D('',#26415,#21075,#21076);
#18443=AXIS2_PLACEMENT_3D('',#26418,#21077,#21078);
#18444=AXIS2_PLACEMENT_3D('',#26421,#21080,#21081);
#18445=AXIS2_PLACEMENT_3D('',#26423,#21083,#21084);
#18446=AXIS2_PLACEMENT_3D('',#26425,#21085,#21086);
#18447=AXIS2_PLACEMENT_3D('',#26426,#21087,#21088);
#18448=AXIS2_PLACEMENT_3D('',#26427,#21089,#21090);
#18449=AXIS2_PLACEMENT_3D('',#26429,#21091,#21092);
#18450=AXIS2_PLACEMENT_3D('',#26430,#21093,#21094);
#18451=AXIS2_PLACEMENT_3D('',#26431,#21095,#21096);
#18452=AXIS2_PLACEMENT_3D('',#26434,#21099,#21100);
#18453=AXIS2_PLACEMENT_3D('',#26435,#21101,#21102);
#18454=AXIS2_PLACEMENT_3D('',#26436,#21103,#21104);
#18455=AXIS2_PLACEMENT_3D('',#26457,#21108,#21109);
#18456=AXIS2_PLACEMENT_3D('',#26460,#21112,#21113);
#18457=AXIS2_PLACEMENT_3D('',#26482,#21116,#21117);
#18458=AXIS2_PLACEMENT_3D('',#26483,#21118,#21119);
#18459=AXIS2_PLACEMENT_3D('',#26486,#21120,#21121);
#18460=AXIS2_PLACEMENT_3D('',#26487,#21122,#21123);
#18461=AXIS2_PLACEMENT_3D('',#26488,#21124,#21125);
#18462=AXIS2_PLACEMENT_3D('',#26489,#21126,#21127);
#18463=AXIS2_PLACEMENT_3D('',#26508,#21128,#21129);
#18464=AXIS2_PLACEMENT_3D('',#26509,#21130,#21131);
#18465=AXIS2_PLACEMENT_3D('',#26510,#21132,#21133);
#18466=AXIS2_PLACEMENT_3D('',#26529,#21134,#21135);
#18467=AXIS2_PLACEMENT_3D('',#26530,#21136,#21137);
#18468=AXIS2_PLACEMENT_3D('',#26531,#21138,#21139);
#18469=AXIS2_PLACEMENT_3D('',#26533,#21140,#21141);
#18470=AXIS2_PLACEMENT_3D('',#26534,#21142,#21143);
#18471=AXIS2_PLACEMENT_3D('',#26535,#21144,#21145);
#18472=AXIS2_PLACEMENT_3D('',#26538,#21148,#21149);
#18473=AXIS2_PLACEMENT_3D('',#26561,#21153,#21154);
#18474=AXIS2_PLACEMENT_3D('',#26564,#21156,#21157);
#18475=AXIS2_PLACEMENT_3D('',#26568,#21160,#21161);
#18476=AXIS2_PLACEMENT_3D('',#26571,#21163,#21164);
#18477=AXIS2_PLACEMENT_3D('',#26573,#21166,#21167);
#18478=AXIS2_PLACEMENT_3D('',#26576,#21168,#21169);
#18479=AXIS2_PLACEMENT_3D('',#26596,#21172,#21173);
#18480=AXIS2_PLACEMENT_3D('',#26613,#21174,#21175);
#18481=AXIS2_PLACEMENT_3D('',#26614,#21176,#21177);
#18482=AXIS2_PLACEMENT_3D('',#26615,#21178,#21179);
#18483=AXIS2_PLACEMENT_3D('',#26617,#21180,#21181);
#18484=AXIS2_PLACEMENT_3D('',#26618,#21182,#21183);
#18485=AXIS2_PLACEMENT_3D('',#26619,#21184,#21185);
#18486=AXIS2_PLACEMENT_3D('',#26621,#21186,#21187);
#18487=AXIS2_PLACEMENT_3D('',#26623,#21188,#21189);
#18488=AXIS2_PLACEMENT_3D('',#26640,#21190,#21191);
#18489=AXIS2_PLACEMENT_3D('',#26642,#21192,#21193);
#18490=AXIS2_PLACEMENT_3D('',#26647,#21197,#21198);
#18491=AXIS2_PLACEMENT_3D('',#26648,#21199,#21200);
#18492=AXIS2_PLACEMENT_3D('',#26649,#21201,#21202);
#18493=AXIS2_PLACEMENT_3D('',#26652,#21205,#21206);
#18494=AXIS2_PLACEMENT_3D('',#26655,#21207,#21208);
#18495=AXIS2_PLACEMENT_3D('',#26656,#21209,#21210);
#18496=AXIS2_PLACEMENT_3D('',#26657,#21211,#21212);
#18497=AXIS2_PLACEMENT_3D('',#26658,#21213,#21214);
#18498=AXIS2_PLACEMENT_3D('',#26661,#21216,#21217);
#18499=AXIS2_PLACEMENT_3D('',#26663,#21219,#21220);
#18500=AXIS2_PLACEMENT_3D('',#26665,#21221,#21222);
#18501=AXIS2_PLACEMENT_3D('',#26666,#21223,#21224);
#18502=AXIS2_PLACEMENT_3D('',#26667,#21225,#21226);
#18503=AXIS2_PLACEMENT_3D('',#26669,#21227,#21228);
#18504=AXIS2_PLACEMENT_3D('',#26670,#21229,#21230);
#18505=AXIS2_PLACEMENT_3D('',#26671,#21231,#21232);
#18506=AXIS2_PLACEMENT_3D('',#26674,#21235,#21236);
#18507=AXIS2_PLACEMENT_3D('',#26676,#21237,#21238);
#18508=AXIS2_PLACEMENT_3D('',#26677,#21239,#21240);
#18509=AXIS2_PLACEMENT_3D('',#26678,#21241,#21242);
#18510=AXIS2_PLACEMENT_3D('',#26699,#21246,#21247);
#18511=AXIS2_PLACEMENT_3D('',#26702,#21250,#21251);
#18512=AXIS2_PLACEMENT_3D('',#26724,#21254,#21255);
#18513=AXIS2_PLACEMENT_3D('',#26725,#21256,#21257);
#18514=AXIS2_PLACEMENT_3D('',#26726,#21258,#21259);
#18515=AXIS2_PLACEMENT_3D('',#26728,#21260,#21261);
#18516=AXIS2_PLACEMENT_3D('',#26729,#21262,#21263);
#18517=AXIS2_PLACEMENT_3D('',#26730,#21264,#21265);
#18518=AXIS2_PLACEMENT_3D('',#26732,#21266,#21267);
#18519=AXIS2_PLACEMENT_3D('',#26733,#21268,#21269);
#18520=AXIS2_PLACEMENT_3D('',#26734,#21270,#21271);
#18521=AXIS2_PLACEMENT_3D('',#26753,#21272,#21273);
#18522=AXIS2_PLACEMENT_3D('',#26754,#21274,#21275);
#18523=AXIS2_PLACEMENT_3D('',#26755,#21276,#21277);
#18524=AXIS2_PLACEMENT_3D('',#26774,#21278,#21279);
#18525=AXIS2_PLACEMENT_3D('',#26775,#21280,#21281);
#18526=AXIS2_PLACEMENT_3D('',#26776,#21282,#21283);
#18527=AXIS2_PLACEMENT_3D('',#26779,#21286,#21287);
#18528=AXIS2_PLACEMENT_3D('',#26784,#21291,#21292);
#18529=AXIS2_PLACEMENT_3D('',#26786,#21293,#21294);
#18530=AXIS2_PLACEMENT_3D('',#26789,#21297,#21298);
#18531=AXIS2_PLACEMENT_3D('',#26791,#21299,#21300);
#18532=AXIS2_PLACEMENT_3D('',#26793,#21301,#21302);
#18533=AXIS2_PLACEMENT_3D('',#26794,#21303,#21304);
#18534=AXIS2_PLACEMENT_3D('',#26795,#21305,#21306);
#18535=AXIS2_PLACEMENT_3D('',#26798,#21309,#21310);
#18536=AXIS2_PLACEMENT_3D('',#26799,#21311,#21312);
#18537=AXIS2_PLACEMENT_3D('',#26800,#21313,#21314);
#18538=AXIS2_PLACEMENT_3D('',#26803,#21317,#21318);
#18539=AXIS2_PLACEMENT_3D('',#26804,#21319,#21320);
#18540=AXIS2_PLACEMENT_3D('',#26805,#21321,#21322);
#18541=AXIS2_PLACEMENT_3D('',#26808,#21325,#21326);
#18542=AXIS2_PLACEMENT_3D('',#26809,#21327,#21328);
#18543=AXIS2_PLACEMENT_3D('',#26810,#21329,#21330);
#18544=AXIS2_PLACEMENT_3D('',#26813,#21333,#21334);
#18545=AXIS2_PLACEMENT_3D('',#26814,#21335,#21336);
#18546=AXIS2_PLACEMENT_3D('',#26815,#21337,#21338);
#18547=AXIS2_PLACEMENT_3D('',#26818,#21341,#21342);
#18548=AXIS2_PLACEMENT_3D('',#26819,#21343,#21344);
#18549=AXIS2_PLACEMENT_3D('',#26820,#21345,#21346);
#18550=AXIS2_PLACEMENT_3D('',#26822,#21347,#21348);
#18551=AXIS2_PLACEMENT_3D('',#26823,#21349,#21350);
#18552=AXIS2_PLACEMENT_3D('',#26825,#21351,#21352);
#18553=AXIS2_PLACEMENT_3D('',#26826,#21353,#21354);
#18554=AXIS2_PLACEMENT_3D('',#26827,#21355,#21356);
#18555=AXIS2_PLACEMENT_3D('',#26829,#21358,#21359);
#18556=AXIS2_PLACEMENT_3D('',#26831,#21361,#21362);
#18557=AXIS2_PLACEMENT_3D('',#26832,#21363,#21364);
#18558=AXIS2_PLACEMENT_3D('',#26834,#21366,#21367);
#18559=AXIS2_PLACEMENT_3D('',#26835,#21368,#21369);
#18560=AXIS2_PLACEMENT_3D('',#26837,#21371,#21372);
#18561=AXIS2_PLACEMENT_3D('',#26838,#21373,#21374);
#18562=AXIS2_PLACEMENT_3D('',#26839,#21375,#21376);
#18563=AXIS2_PLACEMENT_3D('',#26840,#21377,#21378);
#18564=AXIS2_PLACEMENT_3D('',#26841,#21379,#21380);
#18565=AXIS2_PLACEMENT_3D('',#26842,#21381,#21382);
#18566=AXIS2_PLACEMENT_3D('',#26845,#21383,#21384);
#18567=AXIS2_PLACEMENT_3D('',#26849,#21386,#21387);
#18568=AXIS2_PLACEMENT_3D('',#26851,#21389,#21390);
#18569=AXIS2_PLACEMENT_3D('',#26854,#21391,#21392);
#18570=AXIS2_PLACEMENT_3D('',#26858,#21394,#21395);
#18571=AXIS2_PLACEMENT_3D('',#26860,#21397,#21398);
#18572=AXIS2_PLACEMENT_3D('',#26863,#21399,#21400);
#18573=AXIS2_PLACEMENT_3D('',#26867,#21402,#21403);
#18574=AXIS2_PLACEMENT_3D('',#26869,#21405,#21406);
#18575=AXIS2_PLACEMENT_3D('',#26872,#21407,#21408);
#18576=AXIS2_PLACEMENT_3D('',#26876,#21410,#21411);
#18577=AXIS2_PLACEMENT_3D('',#26878,#21413,#21414);
#18578=AXIS2_PLACEMENT_3D('',#26881,#21415,#21416);
#18579=AXIS2_PLACEMENT_3D('',#26885,#21418,#21419);
#18580=AXIS2_PLACEMENT_3D('',#26887,#21421,#21422);
#18581=AXIS2_PLACEMENT_3D('',#26890,#21423,#21424);
#18582=AXIS2_PLACEMENT_3D('',#26894,#21426,#21427);
#18583=AXIS2_PLACEMENT_3D('',#26896,#21429,#21430);
#18584=AXIS2_PLACEMENT_3D('',#26899,#21431,#21432);
#18585=AXIS2_PLACEMENT_3D('',#26900,#21433,#21434);
#18586=AXIS2_PLACEMENT_3D('',#26903,#21436,#21437);
#18587=AXIS2_PLACEMENT_3D('',#26904,#21438,#21439);
#18588=AXIS2_PLACEMENT_3D('',#26907,#21440,#21441);
#18589=AXIS2_PLACEMENT_3D('',#26908,#21442,#21443);
#18590=AXIS2_PLACEMENT_3D('',#26911,#21445,#21446);
#18591=AXIS2_PLACEMENT_3D('',#26912,#21447,#21448);
#18592=AXIS2_PLACEMENT_3D('',#26915,#21449,#21450);
#18593=AXIS2_PLACEMENT_3D('',#26916,#21451,#21452);
#18594=AXIS2_PLACEMENT_3D('',#26919,#21454,#21455);
#18595=AXIS2_PLACEMENT_3D('',#26920,#21456,#21457);
#18596=AXIS2_PLACEMENT_3D('',#26923,#21458,#21459);
#18597=AXIS2_PLACEMENT_3D('',#26924,#21460,#21461);
#18598=AXIS2_PLACEMENT_3D('',#26927,#21463,#21464);
#18599=AXIS2_PLACEMENT_3D('',#26928,#21465,#21466);
#18600=AXIS2_PLACEMENT_3D('',#26931,#21467,#21468);
#18601=AXIS2_PLACEMENT_3D('',#26932,#21469,#21470);
#18602=AXIS2_PLACEMENT_3D('',#26935,#21472,#21473);
#18603=AXIS2_PLACEMENT_3D('',#26936,#21474,#21475);
#18604=AXIS2_PLACEMENT_3D('',#26939,#21476,#21477);
#18605=AXIS2_PLACEMENT_3D('',#26940,#21478,#21479);
#18606=AXIS2_PLACEMENT_3D('',#26943,#21481,#21482);
#18607=AXIS2_PLACEMENT_3D('',#26944,#21483,#21484);
#18608=AXIS2_PLACEMENT_3D('',#26947,#21485,#21486);
#18609=AXIS2_PLACEMENT_3D('',#26948,#21487,#21488);
#18610=AXIS2_PLACEMENT_3D('',#26951,#21490,#21491);
#18611=AXIS2_PLACEMENT_3D('',#26952,#21492,#21493);
#18612=AXIS2_PLACEMENT_3D('',#26955,#21494,#21495);
#18613=AXIS2_PLACEMENT_3D('',#26956,#21496,#21497);
#18614=AXIS2_PLACEMENT_3D('',#26959,#21499,#21500);
#18615=AXIS2_PLACEMENT_3D('',#26960,#21501,#21502);
#18616=AXIS2_PLACEMENT_3D('',#26963,#21503,#21504);
#18617=AXIS2_PLACEMENT_3D('',#26964,#21505,#21506);
#18618=AXIS2_PLACEMENT_3D('',#26967,#21508,#21509);
#18619=AXIS2_PLACEMENT_3D('',#26968,#21510,#21511);
#18620=AXIS2_PLACEMENT_3D('',#26971,#21512,#21513);
#18621=AXIS2_PLACEMENT_3D('',#26972,#21514,#21515);
#18622=AXIS2_PLACEMENT_3D('',#26975,#21517,#21518);
#18623=AXIS2_PLACEMENT_3D('',#26976,#21519,#21520);
#18624=AXIS2_PLACEMENT_3D('',#26979,#21521,#21522);
#18625=AXIS2_PLACEMENT_3D('',#26980,#21523,#21524);
#18626=AXIS2_PLACEMENT_3D('',#26983,#21526,#21527);
#18627=AXIS2_PLACEMENT_3D('',#26984,#21528,#21529);
#18628=AXIS2_PLACEMENT_3D('',#26987,#21530,#21531);
#18629=AXIS2_PLACEMENT_3D('',#26988,#21532,#21533);
#18630=AXIS2_PLACEMENT_3D('',#26991,#21535,#21536);
#18631=AXIS2_PLACEMENT_3D('',#26992,#21537,#21538);
#18632=AXIS2_PLACEMENT_3D('',#26995,#21539,#21540);
#18633=AXIS2_PLACEMENT_3D('',#26996,#21541,#21542);
#18634=AXIS2_PLACEMENT_3D('',#26999,#21544,#21545);
#18635=AXIS2_PLACEMENT_3D('',#27000,#21546,#21547);
#18636=AXIS2_PLACEMENT_3D('',#27009,#21552,#21553);
#18637=AXIS2_PLACEMENT_3D('',#27012,#21554,#21555);
#18638=AXIS2_PLACEMENT_3D('',#27018,#21558,#21559);
#18639=AXIS2_PLACEMENT_3D('',#27022,#21561,#21562);
#18640=AXIS2_PLACEMENT_3D('',#27028,#21566,#21567);
#18641=AXIS2_PLACEMENT_3D('',#27037,#21572,#21573);
#18642=AXIS2_PLACEMENT_3D('',#27045,#21578,#21579);
#18643=AXIS2_PLACEMENT_3D('',#27049,#21582,#21583);
#18644=AXIS2_PLACEMENT_3D('',#27055,#21587,#21588);
#18645=AXIS2_PLACEMENT_3D('',#27060,#21591,#21592);
#18646=AXIS2_PLACEMENT_3D('',#27061,#21593,#21594);
#18647=AXIS2_PLACEMENT_3D('',#27066,#21597,#21598);
#18648=AXIS2_PLACEMENT_3D('',#27068,#21600,#21601);
#18649=AXIS2_PLACEMENT_3D('',#27071,#21602,#21603);
#18650=AXIS2_PLACEMENT_3D('',#27075,#21605,#21606);
#18651=AXIS2_PLACEMENT_3D('',#27077,#21608,#21609);
#18652=AXIS2_PLACEMENT_3D('',#27082,#21612,#21613);
#18653=AXIS2_PLACEMENT_3D('',#27084,#21615,#21616);
#18654=AXIS2_PLACEMENT_3D('',#27095,#21623,#21624);
#18655=AXIS2_PLACEMENT_3D('',#27097,#21626,#21627);
#18656=AXIS2_PLACEMENT_3D('',#27099,#21629,#21630);
#18657=AXIS2_PLACEMENT_3D('',#27100,#21631,#21632);
#18658=AXIS2_PLACEMENT_3D('',#27103,#21635,#21636);
#18659=AXIS2_PLACEMENT_3D('',#27106,#21639,#21640);
#18660=AXIS2_PLACEMENT_3D('',#27109,#21643,#21644);
#18661=AXIS2_PLACEMENT_3D('',#27112,#21647,#21648);
#18662=AXIS2_PLACEMENT_3D('',#27115,#21650,#21651);
#18663=AXIS2_PLACEMENT_3D('',#27116,#21652,#21653);
#18664=AXIS2_PLACEMENT_3D('',#27118,#21654,#21655);
#18665=AXIS2_PLACEMENT_3D('',#27121,#21657,#21658);
#18666=AXIS2_PLACEMENT_3D('',#27122,#21659,#21660);
#18667=AXIS2_PLACEMENT_3D('',#27125,#21662,#21663);
#18668=AXIS2_PLACEMENT_3D('',#27126,#21664,#21665);
#18669=AXIS2_PLACEMENT_3D('',#27129,#21667,#21668);
#18670=AXIS2_PLACEMENT_3D('',#27130,#21669,#21670);
#18671=AXIS2_PLACEMENT_3D('',#27133,#21672,#21673);
#18672=AXIS2_PLACEMENT_3D('',#27134,#21674,#21675);
#18673=AXIS2_PLACEMENT_3D('',#27136,#21676,#21677);
#18674=AXIS2_PLACEMENT_3D('',#27139,#21679,#21680);
#18675=AXIS2_PLACEMENT_3D('',#27140,#21681,#21682);
#18676=AXIS2_PLACEMENT_3D('',#27142,#21683,#21684);
#18677=AXIS2_PLACEMENT_3D('',#27145,#21686,#21687);
#18678=AXIS2_PLACEMENT_3D('',#27146,#21688,#21689);
#18679=AXIS2_PLACEMENT_3D('',#27149,#21691,#21692);
#18680=AXIS2_PLACEMENT_3D('',#27150,#21693,#21694);
#18681=AXIS2_PLACEMENT_3D('',#27153,#21696,#21697);
#18682=AXIS2_PLACEMENT_3D('',#27154,#21698,#21699);
#18683=AXIS2_PLACEMENT_3D('',#27157,#21701,#21702);
#18684=AXIS2_PLACEMENT_3D('',#27158,#21703,#21704);
#18685=AXIS2_PLACEMENT_3D('',#27161,#21706,#21707);
#18686=AXIS2_PLACEMENT_3D('',#27162,#21708,#21709);
#18687=AXIS2_PLACEMENT_3D('',#27165,#21711,#21712);
#18688=AXIS2_PLACEMENT_3D('',#27166,#21713,#21714);
#18689=AXIS2_PLACEMENT_3D('',#27169,#21716,#21717);
#18690=AXIS2_PLACEMENT_3D('',#27170,#21718,#21719);
#18691=AXIS2_PLACEMENT_3D('',#27173,#21721,#21722);
#18692=AXIS2_PLACEMENT_3D('',#27174,#21723,#21724);
#18693=AXIS2_PLACEMENT_3D('',#27177,#21726,#21727);
#18694=AXIS2_PLACEMENT_3D('',#27178,#21728,#21729);
#18695=AXIS2_PLACEMENT_3D('',#27181,#21731,#21732);
#18696=AXIS2_PLACEMENT_3D('',#27182,#21733,#21734);
#18697=AXIS2_PLACEMENT_3D('',#27191,#21739,#21740);
#18698=AXIS2_PLACEMENT_3D('',#27197,#21744,#21745);
#18699=AXIS2_PLACEMENT_3D('',#27200,#21748,#21749);
#18700=AXIS2_PLACEMENT_3D('',#27206,#21753,#21754);
#18701=AXIS2_PLACEMENT_3D('',#27208,#21755,#21756);
#18702=AXIS2_PLACEMENT_3D('',#27210,#21757,#21758);
#18703=AXIS2_PLACEMENT_3D('',#27212,#21760,#21761);
#18704=AXIS2_PLACEMENT_3D('',#27215,#21764,#21765);
#18705=AXIS2_PLACEMENT_3D('',#27221,#21769,#21770);
#18706=AXIS2_PLACEMENT_3D('',#27223,#21771,#21772);
#18707=AXIS2_PLACEMENT_3D('',#27225,#21773,#21774);
#18708=AXIS2_PLACEMENT_3D('',#27227,#21776,#21777);
#18709=AXIS2_PLACEMENT_3D('',#27233,#21781,#21782);
#18710=AXIS2_PLACEMENT_3D('',#27235,#21783,#21784);
#18711=AXIS2_PLACEMENT_3D('',#27237,#21785,#21786);
#18712=AXIS2_PLACEMENT_3D('',#27239,#21788,#21789);
#18713=AXIS2_PLACEMENT_3D('',#27245,#21793,#21794);
#18714=AXIS2_PLACEMENT_3D('',#27254,#21801,#21802);
#18715=AXIS2_PLACEMENT_3D('',#27258,#21805,#21806);
#18716=AXIS2_PLACEMENT_3D('',#27269,#21813,#21814);
#18717=AXIS2_PLACEMENT_3D('',#27275,#21818,#21819);
#18718=AXIS2_PLACEMENT_3D('',#27281,#21823,#21824);
#18719=AXIS2_PLACEMENT_3D('',#27284,#21827,#21828);
#18720=AXIS2_PLACEMENT_3D('',#27286,#21830,#21831);
#18721=AXIS2_PLACEMENT_3D('',#27289,#21834,#21835);
#18722=AXIS2_PLACEMENT_3D('',#27290,#21836,#21837);
#18723=AXIS2_PLACEMENT_3D('',#27291,#21838,#21839);
#18724=AXIS2_PLACEMENT_3D('',#27293,#21841,#21842);
#18725=AXIS2_PLACEMENT_3D('',#27295,#21844,#21845);
#18726=AXIS2_PLACEMENT_3D('',#27296,#21846,#21847);
#18727=AXIS2_PLACEMENT_3D('',#27297,#21848,#21849);
#18728=AXIS2_PLACEMENT_3D('',#27300,#21850,#21851);
#18729=AXIS2_PLACEMENT_3D('',#27304,#21853,#21854);
#18730=AXIS2_PLACEMENT_3D('',#27306,#21856,#21857);
#18731=AXIS2_PLACEMENT_3D('',#27309,#21858,#21859);
#18732=AXIS2_PLACEMENT_3D('',#27313,#21861,#21862);
#18733=AXIS2_PLACEMENT_3D('',#27315,#21864,#21865);
#18734=AXIS2_PLACEMENT_3D('',#27348,#21869,#21870);
#18735=AXIS2_PLACEMENT_3D('',#27350,#21871,#21872);
#18736=AXIS2_PLACEMENT_3D('',#27352,#21873,#21874);
#18737=AXIS2_PLACEMENT_3D('',#27353,#21875,#21876);
#18738=AXIS2_PLACEMENT_3D('',#27382,#21877,#21878);
#18739=AXIS2_PLACEMENT_3D('',#27384,#21879,#21880);
#18740=AXIS2_PLACEMENT_3D('',#27386,#21881,#21882);
#18741=AXIS2_PLACEMENT_3D('',#27387,#21883,#21884);
#18742=AXIS2_PLACEMENT_3D('',#27388,#21885,#21886);
#18743=AXIS2_PLACEMENT_3D('',#27389,#21887,#21888);
#18744=AXIS2_PLACEMENT_3D('',#27391,#21889,#21890);
#18745=AXIS2_PLACEMENT_3D('',#27393,#21892,#21893);
#18746=AXIS2_PLACEMENT_3D('',#27394,#21894,#21895);
#18747=AXIS2_PLACEMENT_3D('',#27396,#21896,#21897);
#18748=AXIS2_PLACEMENT_3D('',#27398,#21899,#21900);
#18749=AXIS2_PLACEMENT_3D('',#27400,#21902,#21903);
#18750=AXIS2_PLACEMENT_3D('',#27409,#21908,#21909);
#18751=AXIS2_PLACEMENT_3D('',#27415,#21913,#21914);
#18752=AXIS2_PLACEMENT_3D('',#27419,#21917,#21918);
#18753=AXIS2_PLACEMENT_3D('',#27422,#21921,#21922);
#18754=AXIS2_PLACEMENT_3D('',#27424,#21924,#21925);
#18755=AXIS2_PLACEMENT_3D('',#27425,#21926,#21927);
#18756=AXIS2_PLACEMENT_3D('',#27426,#21928,#21929);
#18757=AXIS2_PLACEMENT_3D('',#27435,#21934,#21935);
#18758=AXIS2_PLACEMENT_3D('',#27444,#21940,#21941);
#18759=AXIS2_PLACEMENT_3D('',#27447,#21942,#21943);
#18760=AXIS2_PLACEMENT_3D('',#27451,#21945,#21946);
#18761=AXIS2_PLACEMENT_3D('',#27453,#21948,#21949);
#18762=AXIS2_PLACEMENT_3D('',#27456,#21950,#21951);
#18763=AXIS2_PLACEMENT_3D('',#27460,#21953,#21954);
#18764=AXIS2_PLACEMENT_3D('',#27462,#21956,#21957);
#18765=AXIS2_PLACEMENT_3D('',#27465,#21958,#21959);
#18766=AXIS2_PLACEMENT_3D('',#27469,#21961,#21962);
#18767=AXIS2_PLACEMENT_3D('',#27471,#21964,#21965);
#18768=AXIS2_PLACEMENT_3D('',#27474,#21966,#21967);
#18769=AXIS2_PLACEMENT_3D('',#27478,#21969,#21970);
#18770=AXIS2_PLACEMENT_3D('',#27480,#21972,#21973);
#18771=AXIS2_PLACEMENT_3D('',#27486,#21977,#21978);
#18772=AXIS2_PLACEMENT_3D('',#27489,#21981,#21982);
#18773=AXIS2_PLACEMENT_3D('',#27495,#21986,#21987);
#18774=AXIS2_PLACEMENT_3D('',#27498,#21990,#21991);
#18775=AXIS2_PLACEMENT_3D('',#27515,#22001,#22002);
#18776=AXIS2_PLACEMENT_3D('',#27532,#22012,#22013);
#18777=AXIS2_PLACEMENT_3D('',#27535,#22016,#22017);
#18778=AXIS2_PLACEMENT_3D('',#27537,#22019,#22020);
#18779=AXIS2_PLACEMENT_3D('',#27539,#22022,#22023);
#18780=AXIS2_PLACEMENT_3D('',#27541,#22025,#22026);
#18781=AXIS2_PLACEMENT_3D('',#27543,#22028,#22029);
#18782=AXIS2_PLACEMENT_3D('',#27545,#22031,#22032);
#18783=AXIS2_PLACEMENT_3D('',#27547,#22034,#22035);
#18784=AXIS2_PLACEMENT_3D('',#27549,#22037,#22038);
#18785=AXIS2_PLACEMENT_3D('',#27552,#22041,#22042);
#18786=AXIS2_PLACEMENT_3D('',#27553,#22043,#22044);
#18787=AXIS2_PLACEMENT_3D('',#27554,#22045,#22046);
#18788=AXIS2_PLACEMENT_3D('',#27555,#22047,#22048);
#18789=AXIS2_PLACEMENT_3D('',#27562,#22051,#22052);
#18790=AXIS2_PLACEMENT_3D('',#27581,#22053,#22054);
#18791=AXIS2_PLACEMENT_3D('',#27657,#22056,#22057);
#18792=AXIS2_PLACEMENT_3D('',#27733,#22059,#22060);
#18793=AXIS2_PLACEMENT_3D('',#27811,#22062,#22063);
#18794=AXIS2_PLACEMENT_3D('',#27887,#22065,#22066);
#18795=AXIS2_PLACEMENT_3D('',#27963,#22068,#22069);
#18796=AXIS2_PLACEMENT_3D('',#28039,#22071,#22072);
#18797=AXIS2_PLACEMENT_3D('',#28115,#22074,#22075);
#18798=AXIS2_PLACEMENT_3D('',#28193,#22077,#22078);
#18799=AXIS2_PLACEMENT_3D('',#28269,#22080,#22081);
#18800=AXIS2_PLACEMENT_3D('',#28345,#22083,#22084);
#18801=AXIS2_PLACEMENT_3D('',#28423,#22086,#22087);
#18802=AXIS2_PLACEMENT_3D('',#28499,#22089,#22090);
#18803=AXIS2_PLACEMENT_3D('',#28575,#22092,#22093);
#18804=AXIS2_PLACEMENT_3D('',#28651,#22095,#22096);
#18805=AXIS2_PLACEMENT_3D('',#28729,#22098,#22099);
#18806=AXIS2_PLACEMENT_3D('',#28805,#22101,#22102);
#18807=AXIS2_PLACEMENT_3D('',#28881,#22104,#22105);
#18808=AXIS2_PLACEMENT_3D('',#28919,#22107,#22108);
#18809=AXIS2_PLACEMENT_3D('',#28954,#22109,#22110);
#18810=AXIS2_PLACEMENT_3D('',#28958,#22112,#22113);
#18811=AXIS2_PLACEMENT_3D('',#28960,#22114,#22115);
#18812=AXIS2_PLACEMENT_3D('',#28970,#22117,#22118);
#18813=AXIS2_PLACEMENT_3D('',#28991,#22121,#22122);
#18814=AXIS2_PLACEMENT_3D('',#29021,#22124,#22125);
#18815=AXIS2_PLACEMENT_3D('',#29051,#22127,#22128);
#18816=AXIS2_PLACEMENT_3D('',#29081,#22130,#22131);
#18817=AXIS2_PLACEMENT_3D('',#29111,#22133,#22134);
#18818=AXIS2_PLACEMENT_3D('',#29141,#22136,#22137);
#18819=AXIS2_PLACEMENT_3D('',#29171,#22139,#22140);
#18820=AXIS2_PLACEMENT_3D('',#29201,#22142,#22143);
#18821=AXIS2_PLACEMENT_3D('',#29231,#22145,#22146);
#18822=AXIS2_PLACEMENT_3D('',#29261,#22148,#22149);
#18823=AXIS2_PLACEMENT_3D('',#29291,#22151,#22152);
#18824=AXIS2_PLACEMENT_3D('',#29321,#22154,#22155);
#18825=AXIS2_PLACEMENT_3D('',#29351,#22157,#22158);
#18826=AXIS2_PLACEMENT_3D('',#29381,#22160,#22161);
#18827=AXIS2_PLACEMENT_3D('',#29411,#22163,#22164);
#18828=AXIS2_PLACEMENT_3D('',#29441,#22166,#22167);
#18829=AXIS2_PLACEMENT_3D('',#29471,#22169,#22170);
#18830=AXIS2_PLACEMENT_3D('',#29501,#22172,#22173);
#18831=AXIS2_PLACEMENT_3D('',#29531,#22175,#22176);
#18832=AXIS2_PLACEMENT_3D('',#29552,#22179,#22180);
#18833=AXIS2_PLACEMENT_3D('',#29590,#22182,#22183);
#18834=AXIS2_PLACEMENT_3D('',#29619,#22184,#22185);
#18835=AXIS2_PLACEMENT_3D('',#29695,#22187,#22188);
#18836=AXIS2_PLACEMENT_3D('',#29771,#22190,#22191);
#18837=AXIS2_PLACEMENT_3D('',#29796,#22194,#22195);
#18838=AXIS2_PLACEMENT_3D('',#29834,#22197,#22198);
#18839=AXIS2_PLACEMENT_3D('',#29872,#22200,#22201);
#18840=AXIS2_PLACEMENT_3D('',#29910,#22203,#22204);
#18841=AXIS2_PLACEMENT_3D('',#29948,#22206,#22207);
#18842=AXIS2_PLACEMENT_3D('',#29986,#22209,#22210);
#18843=AXIS2_PLACEMENT_3D('',#30024,#22212,#22213);
#18844=AXIS2_PLACEMENT_3D('',#30062,#22215,#22216);
#18845=AXIS2_PLACEMENT_3D('',#30078,#22218,#22219);
#18846=AXIS2_PLACEMENT_3D('',#30109,#22220,#22221);
#18847=AXIS2_PLACEMENT_3D('',#30187,#22223,#22224);
#18848=AXIS2_PLACEMENT_3D('',#30263,#22226,#22227);
#18849=AXIS2_PLACEMENT_3D('',#30322,#22230,#22231);
#18850=AXIS2_PLACEMENT_3D('',#30395,#22232,#22233);
#18851=AXIS2_PLACEMENT_3D('',#30398,#22234,#22235);
#18852=AXIS2_PLACEMENT_3D('',#30404,#22239,#22240);
#18853=AXIS2_PLACEMENT_3D('',#30412,#22243,#22244);
#18854=AXIS2_PLACEMENT_3D('',#30420,#22247,#22248);
#18855=AXIS2_PLACEMENT_3D('',#30428,#22251,#22252);
#18856=AXIS2_PLACEMENT_3D('',#30436,#22256,#22257);
#18857=AXIS2_PLACEMENT_3D('',#30437,#22258,#22259);
#18858=AXIS2_PLACEMENT_3D('',#30447,#22263,#22264);
#18859=AXIS2_PLACEMENT_3D('',#30453,#22266,#22267);
#18860=AXIS2_PLACEMENT_3D('',#30461,#22270,#22271);
#18861=AXIS2_PLACEMENT_3D('',#30469,#22275,#22276);
#18862=AXIS2_PLACEMENT_3D('',#30470,#22277,#22278);
#18863=AXIS2_PLACEMENT_3D('',#30480,#22282,#22283);
#18864=AXIS2_PLACEMENT_3D('',#30486,#22285,#22286);
#18865=AXIS2_PLACEMENT_3D('',#30494,#22289,#22290);
#18866=AXIS2_PLACEMENT_3D('',#30503,#22294,#22295);
#18867=AXIS2_PLACEMENT_3D('',#30504,#22296,#22297);
#18868=AXIS2_PLACEMENT_3D('',#30505,#22298,#22299);
#18869=AXIS2_PLACEMENT_3D('',#30515,#22303,#22304);
#18870=AXIS2_PLACEMENT_3D('',#30525,#22306,#22307);
#18871=AXIS2_PLACEMENT_3D('',#30533,#22310,#22311);
#18872=AXIS2_PLACEMENT_3D('',#30534,#22312,#22313);
#18873=AXIS2_PLACEMENT_3D('',#30535,#22314,#22315);
#18874=AXIS2_PLACEMENT_3D('',#30536,#22316,#22317);
#18875=AXIS2_PLACEMENT_3D('',#30537,#22318,#22319);
#18876=AXIS2_PLACEMENT_3D('',#30538,#22320,#22321);
#18877=AXIS2_PLACEMENT_3D('',#30540,#22322,#22323);
#18878=AXIS2_PLACEMENT_3D('',#30542,#22325,#22326);
#18879=AXIS2_PLACEMENT_3D('',#30543,#22327,#22328);
#18880=AXIS2_PLACEMENT_3D('',#30544,#22329,#22330);
#18881=AXIS2_PLACEMENT_3D('',#30545,#22331,#22332);
#18882=AXIS2_PLACEMENT_3D('',#30568,#22333,#22334);
#18883=AXIS2_PLACEMENT_3D('',#30570,#22335,#22336);
#18884=AXIS2_PLACEMENT_3D('',#30573,#22338,#22339);
#18885=AXIS2_PLACEMENT_3D('',#30574,#22340,#22341);
#18886=AXIS2_PLACEMENT_3D('',#30576,#22342,#22343);
#18887=AXIS2_PLACEMENT_3D('',#30577,#22344,#22345);
#18888=AXIS2_PLACEMENT_3D('',#30578,#22346,#22347);
#18889=AXIS2_PLACEMENT_3D('',#30579,#22348,#22349);
#18890=AXIS2_PLACEMENT_3D('',#30580,#22350,#22351);
#18891=AXIS2_PLACEMENT_3D('',#30582,#22353,#22354);
#18892=AXIS2_PLACEMENT_3D('',#30583,#22355,#22356);
#18893=AXIS2_PLACEMENT_3D('',#30584,#22357,#22358);
#18894=AXIS2_PLACEMENT_3D('',#30585,#22359,#22360);
#18895=AXIS2_PLACEMENT_3D('',#30586,#22361,#22362);
#18896=AXIS2_PLACEMENT_3D('',#30587,#22363,#22364);
#18897=AXIS2_PLACEMENT_3D('',#30588,#22365,#22366);
#18898=AXIS2_PLACEMENT_3D('',#30589,#22367,#22368);
#18899=AXIS2_PLACEMENT_3D('',#30590,#22369,#22370);
#18900=AXIS2_PLACEMENT_3D('',#30591,#22371,#22372);
#18901=AXIS2_PLACEMENT_3D('',#31194,#22377,#22378);
#18902=AXIS2_PLACEMENT_3D('',#31196,#22380,#22381);
#18903=AXIS2_PLACEMENT_3D('',#31198,#22382,#22383);
#18904=AXIS2_PLACEMENT_3D('',#31199,#22384,#22385);
#18905=AXIS2_PLACEMENT_3D('',#31201,#22386,#22387);
#18906=AXIS2_PLACEMENT_3D('',#31204,#22389,#22390);
#18907=AXIS2_PLACEMENT_3D('',#31205,#22391,#22392);
#18908=AXIS2_PLACEMENT_3D('',#31207,#22394,#22395);
#18909=AXIS2_PLACEMENT_3D('',#31208,#22396,#22397);
#18910=AXIS2_PLACEMENT_3D('',#31209,#22398,#22399);
#18911=AXIS2_PLACEMENT_3D('',#31210,#22400,#22401);
#18912=AXIS2_PLACEMENT_3D('',#31211,#22402,#22403);
#18913=AXIS2_PLACEMENT_3D('',#31212,#22404,#22405);
#18914=AXIS2_PLACEMENT_3D('',#31214,#22406,#22407);
#18915=AXIS2_PLACEMENT_3D('',#31216,#22408,#22409);
#18916=AXIS2_PLACEMENT_3D('',#31218,#22410,#22411);
#18917=AXIS2_PLACEMENT_3D('',#31219,#22412,#22413);
#18918=AXIS2_PLACEMENT_3D('',#31220,#22414,#22415);
#18919=AXIS2_PLACEMENT_3D('',#31222,#22416,#22417);
#18920=AXIS2_PLACEMENT_3D('',#31225,#22419,#22420);
#18921=AXIS2_PLACEMENT_3D('',#31226,#22421,#22422);
#18922=AXIS2_PLACEMENT_3D('',#31228,#22423,#22424);
#18923=AXIS2_PLACEMENT_3D('',#31231,#22426,#22427);
#18924=AXIS2_PLACEMENT_3D('',#31232,#22428,#22429);
#18925=AXIS2_PLACEMENT_3D('',#31233,#22430,#22431);
#18926=AXIS2_PLACEMENT_3D('',#31235,#22432,#22433);
#18927=AXIS2_PLACEMENT_3D('',#31236,#22434,#22435);
#18928=AXIS2_PLACEMENT_3D('',#31239,#22436,#22437);
#18929=AXIS2_PLACEMENT_3D('',#31241,#22438,#22439);
#18930=AXIS2_PLACEMENT_3D('',#31243,#22440,#22441);
#18931=AXIS2_PLACEMENT_3D('',#31245,#22442,#22443);
#18932=AXIS2_PLACEMENT_3D('',#31247,#22444,#22445);
#18933=AXIS2_PLACEMENT_3D('',#31250,#22447,#22448);
#18934=AXIS2_PLACEMENT_3D('',#31252,#22449,#22450);
#18935=AXIS2_PLACEMENT_3D('',#31254,#22451,#22452);
#18936=AXIS2_PLACEMENT_3D('',#31255,#22453,#22454);
#18937=AXIS2_PLACEMENT_3D('',#31256,#22455,#22456);
#18938=AXIS2_PLACEMENT_3D('',#31257,#22457,#22458);
#18939=AXIS2_PLACEMENT_3D('',#31258,#22459,#22460);
#18940=AXIS2_PLACEMENT_3D('',#31260,#22461,#22462);
#18941=AXIS2_PLACEMENT_3D('',#31261,#22463,#22464);
#18942=AXIS2_PLACEMENT_3D('',#31262,#22465,#22466);
#18943=AXIS2_PLACEMENT_3D('',#31263,#22467,#22468);
#18944=AXIS2_PLACEMENT_3D('',#31264,#22469,#22470);
#18945=AXIS2_PLACEMENT_3D('',#31265,#22471,#22472);
#18946=AXIS2_PLACEMENT_3D('',#31266,#22473,#22474);
#18947=AXIS2_PLACEMENT_3D('',#31267,#22475,#22476);
#18948=AXIS2_PLACEMENT_3D('',#31268,#22477,#22478);
#18949=AXIS2_PLACEMENT_3D('',#31270,#22479,#22480);
#18950=AXIS2_PLACEMENT_3D('',#31272,#22482,#22483);
#18951=AXIS2_PLACEMENT_3D('',#31273,#22484,#22485);
#18952=AXIS2_PLACEMENT_3D('',#31275,#22486,#22487);
#18953=AXIS2_PLACEMENT_3D('',#31278,#22489,#22490);
#18954=AXIS2_PLACEMENT_3D('',#31279,#22491,#22492);
#18955=AXIS2_PLACEMENT_3D('',#31280,#22493,#22494);
#18956=AXIS2_PLACEMENT_3D('',#31282,#22495,#22496);
#18957=AXIS2_PLACEMENT_3D('',#31285,#22498,#22499);
#18958=AXIS2_PLACEMENT_3D('',#31286,#22500,#22501);
#18959=AXIS2_PLACEMENT_3D('',#31287,#22502,#22503);
#18960=AXIS2_PLACEMENT_3D('',#31289,#22504,#22505);
#18961=AXIS2_PLACEMENT_3D('',#31292,#22507,#22508);
#18962=AXIS2_PLACEMENT_3D('',#31293,#22509,#22510);
#18963=AXIS2_PLACEMENT_3D('',#31294,#22511,#22512);
#18964=AXIS2_PLACEMENT_3D('',#31297,#22514,#22515);
#18965=AXIS2_PLACEMENT_3D('',#31298,#22516,#22517);
#18966=AXIS2_PLACEMENT_3D('',#31307,#22522,#22523);
#18967=AXIS2_PLACEMENT_3D('',#31313,#22527,#22528);
#18968=AXIS2_PLACEMENT_3D('',#31319,#22532,#22533);
#18969=AXIS2_PLACEMENT_3D('',#31325,#22537,#22538);
#18970=AXIS2_PLACEMENT_3D('',#31331,#22542,#22543);
#18971=AXIS2_PLACEMENT_3D('',#31337,#22547,#22548);
#18972=AXIS2_PLACEMENT_3D('',#31343,#22552,#22553);
#18973=AXIS2_PLACEMENT_3D('',#31349,#22557,#22558);
#18974=AXIS2_PLACEMENT_3D('',#31355,#22562,#22563);
#18975=AXIS2_PLACEMENT_3D('',#31361,#22567,#22568);
#18976=AXIS2_PLACEMENT_3D('',#31367,#22572,#22573);
#18977=AXIS2_PLACEMENT_3D('',#31373,#22577,#22578);
#18978=AXIS2_PLACEMENT_3D('',#31379,#22582,#22583);
#18979=AXIS2_PLACEMENT_3D('',#31385,#22587,#22588);
#18980=AXIS2_PLACEMENT_3D('',#31391,#22592,#22593);
#18981=AXIS2_PLACEMENT_3D('',#31397,#22597,#22598);
#18982=AXIS2_PLACEMENT_3D('',#31403,#22602,#22603);
#18983=AXIS2_PLACEMENT_3D('',#31409,#22607,#22608);
#18984=AXIS2_PLACEMENT_3D('',#31415,#22612,#22613);
#18985=AXIS2_PLACEMENT_3D('',#31421,#22617,#22618);
#18986=AXIS2_PLACEMENT_3D('',#31427,#22622,#22623);
#18987=AXIS2_PLACEMENT_3D('',#31433,#22627,#22628);
#18988=AXIS2_PLACEMENT_3D('',#31439,#22632,#22633);
#18989=AXIS2_PLACEMENT_3D('',#31445,#22637,#22638);
#18990=AXIS2_PLACEMENT_3D('',#31451,#22642,#22643);
#18991=AXIS2_PLACEMENT_3D('',#31457,#22647,#22648);
#18992=AXIS2_PLACEMENT_3D('',#31463,#22652,#22653);
#18993=AXIS2_PLACEMENT_3D('',#31469,#22657,#22658);
#18994=AXIS2_PLACEMENT_3D('',#31475,#22662,#22663);
#18995=AXIS2_PLACEMENT_3D('',#31481,#22667,#22668);
#18996=AXIS2_PLACEMENT_3D('',#31487,#22672,#22673);
#18997=AXIS2_PLACEMENT_3D('',#31493,#22677,#22678);
#18998=AXIS2_PLACEMENT_3D('',#31499,#22682,#22683);
#18999=AXIS2_PLACEMENT_3D('',#31505,#22687,#22688);
#19000=AXIS2_PLACEMENT_3D('',#31511,#22692,#22693);
#19001=AXIS2_PLACEMENT_3D('',#31517,#22697,#22698);
#19002=AXIS2_PLACEMENT_3D('',#31523,#22702,#22703);
#19003=AXIS2_PLACEMENT_3D('',#31529,#22707,#22708);
#19004=AXIS2_PLACEMENT_3D('',#31535,#22712,#22713);
#19005=AXIS2_PLACEMENT_3D('',#31541,#22717,#22718);
#19006=AXIS2_PLACEMENT_3D('',#31547,#22722,#22723);
#19007=AXIS2_PLACEMENT_3D('',#31553,#22727,#22728);
#19008=AXIS2_PLACEMENT_3D('',#31559,#22732,#22733);
#19009=AXIS2_PLACEMENT_3D('',#31565,#22737,#22738);
#19010=AXIS2_PLACEMENT_3D('',#31571,#22742,#22743);
#19011=AXIS2_PLACEMENT_3D('',#31577,#22747,#22748);
#19012=AXIS2_PLACEMENT_3D('',#31583,#22752,#22753);
#19013=AXIS2_PLACEMENT_3D('',#31589,#22757,#22758);
#19014=AXIS2_PLACEMENT_3D('',#31595,#22762,#22763);
#19015=AXIS2_PLACEMENT_3D('',#31601,#22767,#22768);
#19016=AXIS2_PLACEMENT_3D('',#31607,#22772,#22773);
#19017=AXIS2_PLACEMENT_3D('',#31613,#22777,#22778);
#19018=AXIS2_PLACEMENT_3D('',#31619,#22782,#22783);
#19019=AXIS2_PLACEMENT_3D('',#31625,#22787,#22788);
#19020=AXIS2_PLACEMENT_3D('',#31631,#22792,#22793);
#19021=AXIS2_PLACEMENT_3D('',#31637,#22797,#22798);
#19022=AXIS2_PLACEMENT_3D('',#31643,#22802,#22803);
#19023=AXIS2_PLACEMENT_3D('',#31649,#22807,#22808);
#19024=AXIS2_PLACEMENT_3D('',#31655,#22812,#22813);
#19025=AXIS2_PLACEMENT_3D('',#31661,#22817,#22818);
#19026=AXIS2_PLACEMENT_3D('',#31667,#22822,#22823);
#19027=AXIS2_PLACEMENT_3D('',#31673,#22827,#22828);
#19028=AXIS2_PLACEMENT_3D('',#31679,#22832,#22833);
#19029=AXIS2_PLACEMENT_3D('',#31685,#22837,#22838);
#19030=AXIS2_PLACEMENT_3D('',#31691,#22842,#22843);
#19031=AXIS2_PLACEMENT_3D('',#31697,#22847,#22848);
#19032=AXIS2_PLACEMENT_3D('',#31703,#22852,#22853);
#19033=AXIS2_PLACEMENT_3D('',#31709,#22857,#22858);
#19034=AXIS2_PLACEMENT_3D('',#31715,#22862,#22863);
#19035=AXIS2_PLACEMENT_3D('',#31721,#22867,#22868);
#19036=AXIS2_PLACEMENT_3D('',#31727,#22872,#22873);
#19037=AXIS2_PLACEMENT_3D('',#31733,#22877,#22878);
#19038=AXIS2_PLACEMENT_3D('',#31739,#22882,#22883);
#19039=AXIS2_PLACEMENT_3D('',#31745,#22887,#22888);
#19040=AXIS2_PLACEMENT_3D('',#31751,#22892,#22893);
#19041=AXIS2_PLACEMENT_3D('',#31757,#22897,#22898);
#19042=AXIS2_PLACEMENT_3D('',#31763,#22902,#22903);
#19043=AXIS2_PLACEMENT_3D('',#31769,#22907,#22908);
#19044=AXIS2_PLACEMENT_3D('',#31775,#22912,#22913);
#19045=AXIS2_PLACEMENT_3D('',#31781,#22917,#22918);
#19046=AXIS2_PLACEMENT_3D('',#31787,#22922,#22923);
#19047=AXIS2_PLACEMENT_3D('',#31793,#22927,#22928);
#19048=AXIS2_PLACEMENT_3D('',#31799,#22932,#22933);
#19049=AXIS2_PLACEMENT_3D('',#31805,#22937,#22938);
#19050=AXIS2_PLACEMENT_3D('',#31811,#22942,#22943);
#19051=AXIS2_PLACEMENT_3D('',#31817,#22947,#22948);
#19052=AXIS2_PLACEMENT_3D('',#31823,#22952,#22953);
#19053=AXIS2_PLACEMENT_3D('',#31829,#22957,#22958);
#19054=AXIS2_PLACEMENT_3D('',#31835,#22962,#22963);
#19055=AXIS2_PLACEMENT_3D('',#31838,#22966,#22967);
#19056=AXIS2_PLACEMENT_3D('',#31839,#22968,#22969);
#19057=AXIS2_PLACEMENT_3D('',#31840,#22970,#22971);
#19058=AXIS2_PLACEMENT_3D('',#31841,#22972,#22973);
#19059=AXIS2_PLACEMENT_3D('',#31843,#22974,#22975);
#19060=AXIS2_PLACEMENT_3D('',#31844,#22976,#22977);
#19061=AXIS2_PLACEMENT_3D('',#31846,#22978,#22979);
#19062=AXIS2_PLACEMENT_3D('',#31847,#22980,#22981);
#19063=AXIS2_PLACEMENT_3D('',#31850,#22982,#22983);
#19064=AXIS2_PLACEMENT_3D('',#31851,#22984,#22985);
#19065=AXIS2_PLACEMENT_3D('',#32397,#22989,#22990);
#19066=AXIS2_PLACEMENT_3D('',#32941,#22993,#22994);
#19067=AXIS2_PLACEMENT_3D('',#32942,#22995,#22996);
#19068=AXIS2_PLACEMENT_3D('',#32944,#22998,#22999);
#19069=AXIS2_PLACEMENT_3D('',#32945,#23000,#23001);
#19070=AXIS2_PLACEMENT_3D('',#32946,#23002,#23003);
#19071=AXIS2_PLACEMENT_3D('',#32947,#23004,#23005);
#19072=AXIS2_PLACEMENT_3D('',#32948,#23006,#23007);
#19073=AXIS2_PLACEMENT_3D('',#32951,#23009,#23010);
#19074=AXIS2_PLACEMENT_3D('',#32952,#23011,#23012);
#19075=AXIS2_PLACEMENT_3D('',#32955,#23014,#23015);
#19076=AXIS2_PLACEMENT_3D('',#32956,#23016,#23017);
#19077=AXIS2_PLACEMENT_3D('',#32959,#23019,#23020);
#19078=AXIS2_PLACEMENT_3D('',#32960,#23021,#23022);
#19079=AXIS2_PLACEMENT_3D('',#32962,#23023,#23024);
#19080=AXIS2_PLACEMENT_3D('',#32965,#23026,#23027);
#19081=AXIS2_PLACEMENT_3D('',#32966,#23028,#23029);
#19082=AXIS2_PLACEMENT_3D('',#32968,#23031,#23032);
#19083=AXIS2_PLACEMENT_3D('',#32969,#23033,#23034);
#19084=AXIS2_PLACEMENT_3D('',#32970,#23035,#23036);
#19085=AXIS2_PLACEMENT_3D('',#32971,#23037,#23038);
#19086=AXIS2_PLACEMENT_3D('',#32972,#23039,#23040);
#19087=AXIS2_PLACEMENT_3D('',#32974,#23041,#23042);
#19088=AXIS2_PLACEMENT_3D('',#32977,#23044,#23045);
#19089=AXIS2_PLACEMENT_3D('',#32978,#23046,#23047);
#19090=AXIS2_PLACEMENT_3D('',#32983,#23049,#23050);
#19091=AXIS2_PLACEMENT_3D('',#32984,#23051,#23052);
#19092=AXIS2_PLACEMENT_3D('',#32985,#23053,#23054);
#19093=AXIS2_PLACEMENT_3D('',#32986,#23055,#23056);
#19094=AXIS2_PLACEMENT_3D('',#32989,#23058,#23059);
#19095=AXIS2_PLACEMENT_3D('',#32990,#23060,#23061);
#19096=AXIS2_PLACEMENT_3D('',#33003,#23068,#23069);
#19097=AXIS2_PLACEMENT_3D('',#33009,#23073,#23074);
#19098=AXIS2_PLACEMENT_3D('',#33013,#23077,#23078);
#19099=AXIS2_PLACEMENT_3D('',#33017,#23081,#23082);
#19100=AXIS2_PLACEMENT_3D('',#33021,#23085,#23086);
#19101=AXIS2_PLACEMENT_3D('',#33025,#23089,#23090);
#19102=AXIS2_PLACEMENT_3D('',#33027,#23092,#23093);
#19103=AXIS2_PLACEMENT_3D('',#33260,#23103,#23104);
#19104=AXIS2_PLACEMENT_3D('',#33264,#23107,#23108);
#19105=AXIS2_PLACEMENT_3D('',#33268,#23111,#23112);
#19106=AXIS2_PLACEMENT_3D('',#33272,#23115,#23116);
#19107=AXIS2_PLACEMENT_3D('',#33276,#23119,#23120);
#19108=AXIS2_PLACEMENT_3D('',#33445,#23126,#23127);
#19109=AXIS2_PLACEMENT_3D('',#33506,#23130,#23131);
#19110=AXIS2_PLACEMENT_3D('',#33517,#23137,#23138);
#19111=AXIS2_PLACEMENT_3D('',#33523,#23142,#23143);
#19112=AXIS2_PLACEMENT_3D('',#33529,#23147,#23148);
#19113=AXIS2_PLACEMENT_3D('',#33538,#23153,#23154);
#19114=AXIS2_PLACEMENT_3D('',#33544,#23158,#23159);
#19115=AXIS2_PLACEMENT_3D('',#33552,#23164,#23165);
#19116=AXIS2_PLACEMENT_3D('',#33561,#23170,#23171);
#19117=AXIS2_PLACEMENT_3D('',#33571,#23177,#23178);
#19118=AXIS2_PLACEMENT_3D('',#33573,#23179,#23180);
#19119=AXIS2_PLACEMENT_3D('',#33574,#23181,#23182);
#19120=AXIS2_PLACEMENT_3D('',#33576,#23183,#23184);
#19121=AXIS2_PLACEMENT_3D('',#33577,#23185,#23186);
#19122=AXIS2_PLACEMENT_3D('',#33579,#23187,#23188);
#19123=AXIS2_PLACEMENT_3D('',#33581,#23190,#23191);
#19124=AXIS2_PLACEMENT_3D('',#33583,#23192,#23193);
#19125=AXIS2_PLACEMENT_3D('',#33585,#23195,#23196);
#19126=AXIS2_PLACEMENT_3D('',#33598,#23203,#23204);
#19127=AXIS2_PLACEMENT_3D('',#33604,#23208,#23209);
#19128=AXIS2_PLACEMENT_3D('',#33614,#23215,#23216);
#19129=AXIS2_PLACEMENT_3D('',#33617,#23219,#23220);
#19130=AXIS2_PLACEMENT_3D('',#33618,#23221,#23222);
#19131=AXIS2_PLACEMENT_3D('',#33621,#23225,#23226);
#19132=AXIS2_PLACEMENT_3D('',#33631,#23231,#23232);
#19133=AXIS2_PLACEMENT_3D('',#33633,#23233,#23234);
#19134=AXIS2_PLACEMENT_3D('',#33634,#23235,#23236);
#19135=AXIS2_PLACEMENT_3D('',#33644,#23241,#23242);
#19136=AXIS2_PLACEMENT_3D('',#33646,#23243,#23244);
#19137=AXIS2_PLACEMENT_3D('',#33647,#23245,#23246);
#19138=AXIS2_PLACEMENT_3D('',#33651,#23250,#23251);
#19139=AXIS2_PLACEMENT_3D('',#33653,#23253,#23254);
#19140=AXIS2_PLACEMENT_3D('',#33655,#23256,#23257);
#19141=AXIS2_PLACEMENT_3D('',#33657,#23259,#23260);
#19142=AXIS2_PLACEMENT_3D('',#33667,#23266,#23267);
#19143=AXIS2_PLACEMENT_3D('',#33669,#23269,#23270);
#19144=AXIS2_PLACEMENT_3D('',#33671,#23271,#23272);
#19145=AXIS2_PLACEMENT_3D('',#33672,#23273,#23274);
#19146=AXIS2_PLACEMENT_3D('',#33674,#23275,#23276);
#19147=AXIS2_PLACEMENT_3D('',#33675,#23277,#23278);
#19148=AXIS2_PLACEMENT_3D('',#33677,#23279,#23280);
#19149=AXIS2_PLACEMENT_3D('',#33679,#23282,#23283);
#19150=AXIS2_PLACEMENT_3D('',#33681,#23284,#23285);
#19151=AXIS2_PLACEMENT_3D('',#33683,#23287,#23288);
#19152=AXIS2_PLACEMENT_3D('',#33693,#23294,#23295);
#19153=AXIS2_PLACEMENT_3D('',#33697,#23298,#23299);
#19154=AXIS2_PLACEMENT_3D('',#33705,#23304,#23305);
#19155=AXIS2_PLACEMENT_3D('',#33708,#23308,#23309);
#19156=AXIS2_PLACEMENT_3D('',#33709,#23310,#23311);
#19157=AXIS2_PLACEMENT_3D('',#33715,#23315,#23316);
#19158=AXIS2_PLACEMENT_3D('',#33728,#23323,#23324);
#19159=AXIS2_PLACEMENT_3D('',#33732,#23328,#23329);
#19160=AXIS2_PLACEMENT_3D('',#33736,#23333,#23334);
#19161=AXIS2_PLACEMENT_3D('',#33740,#23338,#23339);
#19162=AXIS2_PLACEMENT_3D('',#33742,#23341,#23342);
#19163=AXIS2_PLACEMENT_3D('',#33744,#23344,#23345);
#19164=AXIS2_PLACEMENT_3D('',#33747,#23348,#23349);
#19165=AXIS2_PLACEMENT_3D('',#33748,#23350,#23351);
#19166=AXIS2_PLACEMENT_3D('',#33750,#23353,#23354);
#19167=AXIS2_PLACEMENT_3D('',#33751,#23355,#23356);
#19168=AXIS2_PLACEMENT_3D('',#33752,#23357,#23358);
#19169=AXIS2_PLACEMENT_3D('',#33753,#23359,#23360);
#19170=AXIS2_PLACEMENT_3D('',#33755,#23361,#23362);
#19171=AXIS2_PLACEMENT_3D('',#33757,#23363,#23364);
#19172=AXIS2_PLACEMENT_3D('',#33758,#23365,#23366);
#19173=AXIS2_PLACEMENT_3D('',#33761,#23367,#23368);
#19174=AXIS2_PLACEMENT_3D('',#33762,#23369,#23370);
#19175=AXIS2_PLACEMENT_3D('',#33764,#23372,#23373);
#19176=AXIS2_PLACEMENT_3D('',#33766,#23375,#23376);
#19177=AXIS2_PLACEMENT_3D('',#33773,#23379,#23380);
#19178=AXIS2_PLACEMENT_3D('',#33796,#23381,#23382);
#19179=AXIS2_PLACEMENT_3D('',#33872,#23384,#23385);
#19180=AXIS2_PLACEMENT_3D('',#33950,#23387,#23388);
#19181=AXIS2_PLACEMENT_3D('',#34026,#23390,#23391);
#19182=AXIS2_PLACEMENT_3D('',#34102,#23393,#23394);
#19183=AXIS2_PLACEMENT_3D('',#34178,#23396,#23397);
#19184=AXIS2_PLACEMENT_3D('',#34256,#23399,#23400);
#19185=AXIS2_PLACEMENT_3D('',#34332,#23402,#23403);
#19186=AXIS2_PLACEMENT_3D('',#34408,#23405,#23406);
#19187=AXIS2_PLACEMENT_3D('',#34486,#23408,#23409);
#19188=AXIS2_PLACEMENT_3D('',#34562,#23411,#23412);
#19189=AXIS2_PLACEMENT_3D('',#34638,#23414,#23415);
#19190=AXIS2_PLACEMENT_3D('',#34714,#23417,#23418);
#19191=AXIS2_PLACEMENT_3D('',#34719,#23420,#23421);
#19192=AXIS2_PLACEMENT_3D('',#34728,#23422,#23423);
#19193=AXIS2_PLACEMENT_3D('',#34749,#23426,#23427);
#19194=AXIS2_PLACEMENT_3D('',#34779,#23429,#23430);
#19195=AXIS2_PLACEMENT_3D('',#34809,#23432,#23433);
#19196=AXIS2_PLACEMENT_3D('',#34839,#23435,#23436);
#19197=AXIS2_PLACEMENT_3D('',#34869,#23438,#23439);
#19198=AXIS2_PLACEMENT_3D('',#34899,#23441,#23442);
#19199=AXIS2_PLACEMENT_3D('',#34929,#23444,#23445);
#19200=AXIS2_PLACEMENT_3D('',#34959,#23447,#23448);
#19201=AXIS2_PLACEMENT_3D('',#34989,#23450,#23451);
#19202=AXIS2_PLACEMENT_3D('',#35019,#23453,#23454);
#19203=AXIS2_PLACEMENT_3D('',#35049,#23456,#23457);
#19204=AXIS2_PLACEMENT_3D('',#35079,#23459,#23460);
#19205=AXIS2_PLACEMENT_3D('',#35109,#23462,#23463);
#19206=AXIS2_PLACEMENT_3D('',#35130,#23466,#23467);
#19207=AXIS2_PLACEMENT_3D('',#35132,#23468,#23469);
#19208=AXIS2_PLACEMENT_3D('',#35135,#23471,#23472);
#19209=AXIS2_PLACEMENT_3D('',#35136,#23473,#23474);
#19210=AXIS2_PLACEMENT_3D('',#35138,#23475,#23476);
#19211=AXIS2_PLACEMENT_3D('',#35141,#23478,#23479);
#19212=AXIS2_PLACEMENT_3D('',#35142,#23480,#23481);
#19213=AXIS2_PLACEMENT_3D('',#35144,#23482,#23483);
#19214=AXIS2_PLACEMENT_3D('',#35147,#23485,#23486);
#19215=AXIS2_PLACEMENT_3D('',#35148,#23487,#23488);
#19216=AXIS2_PLACEMENT_3D('',#35150,#23489,#23490);
#19217=AXIS2_PLACEMENT_3D('',#35152,#23491,#23492);
#19218=AXIS2_PLACEMENT_3D('',#35154,#23493,#23494);
#19219=AXIS2_PLACEMENT_3D('',#35155,#23495,#23496);
#19220=AXIS2_PLACEMENT_3D('',#35156,#23497,#23498);
#19221=AXIS2_PLACEMENT_3D('',#35159,#23499,#23500);
#19222=AXIS2_PLACEMENT_3D('',#35160,#23501,#23502);
#19223=AXIS2_PLACEMENT_3D('',#35162,#23503,#23504);
#19224=AXIS2_PLACEMENT_3D('',#35163,#23505,#23506);
#19225=AXIS2_PLACEMENT_3D('',#35164,#23507,#23508);
#19226=AXIS2_PLACEMENT_3D('',#35167,#23509,#23510);
#19227=AXIS2_PLACEMENT_3D('',#35168,#23511,#23512);
#19228=AXIS2_PLACEMENT_3D('',#35170,#23513,#23514);
#19229=AXIS2_PLACEMENT_3D('',#35171,#23515,#23516);
#19230=AXIS2_PLACEMENT_3D('',#35172,#23517,#23518);
#19231=AXIS2_PLACEMENT_3D('',#35174,#23519,#23520);
#19232=AXIS2_PLACEMENT_3D('',#35176,#23521,#23522);
#19233=AXIS2_PLACEMENT_3D('',#35178,#23523,#23524);
#19234=AXIS2_PLACEMENT_3D('',#35179,#23525,#23526);
#19235=AXIS2_PLACEMENT_3D('',#35180,#23527,#23528);
#19236=AXIS2_PLACEMENT_3D('',#35182,#23530,#23531);
#19237=AXIS2_PLACEMENT_3D('',#35184,#23533,#23534);
#19238=AXIS2_PLACEMENT_3D('',#35185,#23535,#23536);
#19239=AXIS2_PLACEMENT_3D('',#35187,#23537,#23538);
#19240=AXIS2_PLACEMENT_3D('',#35188,#23539,#23540);
#19241=AXIS2_PLACEMENT_3D('',#35190,#23541,#23542);
#19242=AXIS2_PLACEMENT_3D('',#35191,#23543,#23544);
#19243=AXIS2_PLACEMENT_3D('',#35207,#23545,#23546);
#19244=AXIS2_PLACEMENT_3D('',#35208,#23547,#23548);
#19245=AXIS2_PLACEMENT_3D('',#35599,#23552,#23553);
#19246=AXIS2_PLACEMENT_3D('',#35997,#23556,#23557);
#19247=AXIS2_PLACEMENT_3D('',#35999,#23559,#23560);
#19248=AXIS2_PLACEMENT_3D('',#36000,#23561,#23562);
#19249=AXIS2_PLACEMENT_3D('',#36001,#23563,#23564);
#19250=AXIS2_PLACEMENT_3D('',#36002,#23565,#23566);
#19251=AXIS2_PLACEMENT_3D('',#36005,#23568,#23569);
#19252=AXIS2_PLACEMENT_3D('',#36006,#23570,#23571);
#19253=AXIS2_PLACEMENT_3D('',#36008,#23573,#23574);
#19254=AXIS2_PLACEMENT_3D('',#36011,#23575,#23576);
#19255=AXIS2_PLACEMENT_3D('',#36012,#23577,#23578);
#19256=AXIS2_PLACEMENT_3D('',#36015,#23580,#23581);
#19257=AXIS2_PLACEMENT_3D('',#36016,#23582,#23583);
#19258=AXIS2_PLACEMENT_3D('',#36017,#23584,#23585);
#19259=AXIS2_PLACEMENT_3D('',#36018,#23586,#23587);
#19260=AXIS2_PLACEMENT_3D('',#36019,#23588,#23589);
#19261=AXIS2_PLACEMENT_3D('',#36021,#23590,#23591);
#19262=AXIS2_PLACEMENT_3D('',#36023,#23592,#23593);
#19263=AXIS2_PLACEMENT_3D('',#36024,#23594,#23595);
#19264=AXIS2_PLACEMENT_3D('',#36025,#23596,#23597);
#19265=AXIS2_PLACEMENT_3D('',#36027,#23598,#23599);
#19266=AXIS2_PLACEMENT_3D('',#36029,#23600,#23601);
#19267=AXIS2_PLACEMENT_3D('',#36030,#23602,#23603);
#19268=AXIS2_PLACEMENT_3D('',#36031,#23604,#23605);
#19269=AXIS2_PLACEMENT_3D('',#36033,#23607,#23608);
#19270=AXIS2_PLACEMENT_3D('',#36035,#23609,#23610);
#19271=AXIS2_PLACEMENT_3D('',#36037,#23612,#23613);
#19272=AXIS2_PLACEMENT_3D('',#36040,#23614,#23615);
#19273=AXIS2_PLACEMENT_3D('',#36044,#23617,#23618);
#19274=AXIS2_PLACEMENT_3D('',#36046,#23620,#23621);
#19275=AXIS2_PLACEMENT_3D('',#36048,#23622,#23623);
#19276=AXIS2_PLACEMENT_3D('',#36051,#23625,#23626);
#19277=AXIS2_PLACEMENT_3D('',#36052,#23627,#23628);
#19278=AXIS2_PLACEMENT_3D('',#36069,#23636,#23637);
#19279=AXIS2_PLACEMENT_3D('',#36081,#23644,#23645);
#19280=AXIS2_PLACEMENT_3D('',#36084,#23646,#23647);
#19281=AXIS2_PLACEMENT_3D('',#36088,#23649,#23650);
#19282=AXIS2_PLACEMENT_3D('',#36090,#23652,#23653);
#19283=AXIS2_PLACEMENT_3D('',#36111,#23663,#23664);
#19284=AXIS2_PLACEMENT_3D('',#36120,#23669,#23670);
#19285=AXIS2_PLACEMENT_3D('',#36133,#23677,#23678);
#19286=AXIS2_PLACEMENT_3D('',#36137,#23680,#23681);
#19287=AXIS2_PLACEMENT_3D('',#36140,#23683,#23684);
#19288=AXIS2_PLACEMENT_3D('',#36143,#23686,#23687);
#19289=AXIS2_PLACEMENT_3D('',#36147,#23689,#23690);
#19290=AXIS2_PLACEMENT_3D('',#36149,#23692,#23693);
#19291=AXIS2_PLACEMENT_3D('',#36151,#23695,#23696);
#19292=AXIS2_PLACEMENT_3D('',#36153,#23698,#23699);
#19293=AXIS2_PLACEMENT_3D('',#36155,#23701,#23702);
#19294=AXIS2_PLACEMENT_3D('',#36157,#23704,#23705);
#19295=AXIS2_PLACEMENT_3D('',#36159,#23707,#23708);
#19296=AXIS2_PLACEMENT_3D('',#36161,#23710,#23711);
#19297=AXIS2_PLACEMENT_3D('',#36163,#23713,#23714);
#19298=AXIS2_PLACEMENT_3D('',#36165,#23716,#23717);
#19299=AXIS2_PLACEMENT_3D('',#36167,#23718,#23719);
#19300=AXIS2_PLACEMENT_3D('',#36171,#23721,#23722);
#19301=AXIS2_PLACEMENT_3D('',#36176,#23725,#23726);
#19302=AXIS2_PLACEMENT_3D('',#36179,#23728,#23729);
#19303=AXIS2_PLACEMENT_3D('',#36180,#23730,#23731);
#19304=AXIS2_PLACEMENT_3D('',#36184,#23733,#23734);
#19305=AXIS2_PLACEMENT_3D('',#36187,#23736,#23737);
#19306=AXIS2_PLACEMENT_3D('',#36191,#23739,#23740);
#19307=AXIS2_PLACEMENT_3D('',#36195,#23743,#23744);
#19308=AXIS2_PLACEMENT_3D('',#36196,#23745,#23746);
#19309=AXIS2_PLACEMENT_3D('',#36201,#23748,#23749);
#19310=AXIS2_PLACEMENT_3D('',#36206,#23752,#23753);
#19311=AXIS2_PLACEMENT_3D('',#36209,#23755,#23756);
#19312=AXIS2_PLACEMENT_3D('',#36210,#23757,#23758);
#19313=AXIS2_PLACEMENT_3D('',#36211,#23759,#23760);
#19314=AXIS2_PLACEMENT_3D('',#36213,#23762,#23763);
#19315=AXIS2_PLACEMENT_3D('',#36216,#23766,#23767);
#19316=AXIS2_PLACEMENT_3D('',#36219,#23770,#23771);
#19317=AXIS2_PLACEMENT_3D('',#36221,#23773,#23774);
#19318=AXIS2_PLACEMENT_3D('',#36222,#23775,#23776);
#19319=AXIS2_PLACEMENT_3D('',#36223,#23777,#23778);
#19320=AXIS2_PLACEMENT_3D('',#36224,#23779,#23780);
#19321=AXIS2_PLACEMENT_3D('',#36225,#23781,#23782);
#19322=AXIS2_PLACEMENT_3D('',#36227,#23784,#23785);
#19323=AXIS2_PLACEMENT_3D('',#36230,#23788,#23789);
#19324=AXIS2_PLACEMENT_3D('',#36233,#23792,#23793);
#19325=AXIS2_PLACEMENT_3D('',#36235,#23795,#23796);
#19326=AXIS2_PLACEMENT_3D('',#36236,#23797,#23798);
#19327=AXIS2_PLACEMENT_3D('',#36237,#23799,#23800);
#19328=AXIS2_PLACEMENT_3D('',#36238,#23801,#23802);
#19329=AXIS2_PLACEMENT_3D('',#36239,#23803,#23804);
#19330=AXIS2_PLACEMENT_3D('',#36240,#23805,#23806);
#19331=AXIS2_PLACEMENT_3D('',#36241,#23807,#23808);
#19332=AXIS2_PLACEMENT_3D('',#36247,#23812,#23813);
#19333=AXIS2_PLACEMENT_3D('',#36251,#23816,#23817);
#19334=AXIS2_PLACEMENT_3D('',#36255,#23820,#23821);
#19335=AXIS2_PLACEMENT_3D('',#36259,#23824,#23825);
#19336=AXIS2_PLACEMENT_3D('',#36263,#23828,#23829);
#19337=AXIS2_PLACEMENT_3D('',#36265,#23831,#23832);
#19338=AXIS2_PLACEMENT_3D('',#36278,#23839,#23840);
#19339=AXIS2_PLACEMENT_3D('',#36279,#23841,#23842);
#19340=AXIS2_PLACEMENT_3D('',#36280,#23843,#23844);
#19341=AXIS2_PLACEMENT_3D('',#36281,#23845,#23846);
#19342=AXIS2_PLACEMENT_3D('',#36282,#23847,#23848);
#19343=AXIS2_PLACEMENT_3D('',#36283,#23849,#23850);
#19344=AXIS2_PLACEMENT_3D('',#36284,#23851,#23852);
#19345=AXIS2_PLACEMENT_3D('',#36285,#23853,#23854);
#19346=AXIS2_PLACEMENT_3D('',#36286,#23855,#23856);
#19347=AXIS2_PLACEMENT_3D('',#36287,#23857,#23858);
#19348=AXIS2_PLACEMENT_3D('',#36288,#23859,#23860);
#19349=AXIS2_PLACEMENT_3D('',#36289,#23861,#23862);
#19350=AXIS2_PLACEMENT_3D('',#36290,#23863,#23864);
#19351=AXIS2_PLACEMENT_3D('',#36292,#23866,#23867);
#19352=AXIS2_PLACEMENT_3D('',#36294,#23868,#23869);
#19353=AXIS2_PLACEMENT_3D('',#36295,#23870,#23871);
#19354=AXIS2_PLACEMENT_3D('',#36298,#23873,#23874);
#19355=AXIS2_PLACEMENT_3D('',#36299,#23875,#23876);
#19356=AXIS2_PLACEMENT_3D('',#36308,#23881,#23882);
#19357=AXIS2_PLACEMENT_3D('',#36310,#23883,#23884);
#19358=AXIS2_PLACEMENT_3D('',#36313,#23886,#23887);
#19359=AXIS2_PLACEMENT_3D('',#36314,#23888,#23889);
#19360=AXIS2_PLACEMENT_3D('',#36320,#23893,#23894);
#19361=AXIS2_PLACEMENT_3D('',#36326,#23898,#23899);
#19362=AXIS2_PLACEMENT_3D('',#36332,#23903,#23904);
#19363=AXIS2_PLACEMENT_3D('',#36338,#23908,#23909);
#19364=AXIS2_PLACEMENT_3D('',#36344,#23913,#23914);
#19365=AXIS2_PLACEMENT_3D('',#36350,#23918,#23919);
#19366=AXIS2_PLACEMENT_3D('',#36356,#23923,#23924);
#19367=AXIS2_PLACEMENT_3D('',#36362,#23928,#23929);
#19368=AXIS2_PLACEMENT_3D('',#36368,#23933,#23934);
#19369=AXIS2_PLACEMENT_3D('',#36374,#23938,#23939);
#19370=AXIS2_PLACEMENT_3D('',#36380,#23943,#23944);
#19371=AXIS2_PLACEMENT_3D('',#36386,#23948,#23949);
#19372=AXIS2_PLACEMENT_3D('',#36392,#23953,#23954);
#19373=AXIS2_PLACEMENT_3D('',#36398,#23958,#23959);
#19374=AXIS2_PLACEMENT_3D('',#36404,#23963,#23964);
#19375=AXIS2_PLACEMENT_3D('',#36410,#23968,#23969);
#19376=AXIS2_PLACEMENT_3D('',#36416,#23973,#23974);
#19377=AXIS2_PLACEMENT_3D('',#36422,#23978,#23979);
#19378=AXIS2_PLACEMENT_3D('',#36428,#23983,#23984);
#19379=AXIS2_PLACEMENT_3D('',#36434,#23988,#23989);
#19380=AXIS2_PLACEMENT_3D('',#36440,#23993,#23994);
#19381=AXIS2_PLACEMENT_3D('',#36446,#23998,#23999);
#19382=AXIS2_PLACEMENT_3D('',#36452,#24003,#24004);
#19383=AXIS2_PLACEMENT_3D('',#36458,#24008,#24009);
#19384=AXIS2_PLACEMENT_3D('',#36464,#24013,#24014);
#19385=AXIS2_PLACEMENT_3D('',#36470,#24018,#24019);
#19386=AXIS2_PLACEMENT_3D('',#36476,#24023,#24024);
#19387=AXIS2_PLACEMENT_3D('',#36482,#24028,#24029);
#19388=AXIS2_PLACEMENT_3D('',#36488,#24033,#24034);
#19389=AXIS2_PLACEMENT_3D('',#36494,#24038,#24039);
#19390=AXIS2_PLACEMENT_3D('',#36500,#24043,#24044);
#19391=AXIS2_PLACEMENT_3D('',#36506,#24048,#24049);
#19392=AXIS2_PLACEMENT_3D('',#36512,#24053,#24054);
#19393=AXIS2_PLACEMENT_3D('',#36518,#24058,#24059);
#19394=AXIS2_PLACEMENT_3D('',#36524,#24063,#24064);
#19395=AXIS2_PLACEMENT_3D('',#36530,#24068,#24069);
#19396=AXIS2_PLACEMENT_3D('',#36536,#24073,#24074);
#19397=AXIS2_PLACEMENT_3D('',#36542,#24078,#24079);
#19398=AXIS2_PLACEMENT_3D('',#36544,#24080,#24081);
#19399=AXIS2_PLACEMENT_3D('',#36546,#24082,#24083);
#19400=AXIS2_PLACEMENT_3D('',#36548,#24085,#24086);
#19401=AXIS2_PLACEMENT_3D('',#36554,#24090,#24091);
#19402=AXIS2_PLACEMENT_3D('',#36557,#24094,#24095);
#19403=AXIS2_PLACEMENT_3D('',#36558,#24096,#24097);
#19404=AXIS2_PLACEMENT_3D('',#36559,#24098,#24099);
#19405=AXIS2_PLACEMENT_3D('',#36560,#24100,#24101);
#19406=AXIS2_PLACEMENT_3D('',#36561,#24102,#24103);
#19407=AXIS2_PLACEMENT_3D('',#36563,#24104,#24105);
#19408=AXIS2_PLACEMENT_3D('',#36566,#24107,#24108);
#19409=AXIS2_PLACEMENT_3D('',#36567,#24109,#24110);
#19410=AXIS2_PLACEMENT_3D('',#36576,#24115,#24116);
#19411=AXIS2_PLACEMENT_3D('',#36578,#24117,#24118);
#19412=AXIS2_PLACEMENT_3D('',#36581,#24120,#24121);
#19413=AXIS2_PLACEMENT_3D('',#36582,#24122,#24123);
#19414=AXIS2_PLACEMENT_3D('',#36588,#24127,#24128);
#19415=AXIS2_PLACEMENT_3D('',#36594,#24132,#24133);
#19416=AXIS2_PLACEMENT_3D('',#36600,#24137,#24138);
#19417=AXIS2_PLACEMENT_3D('',#36606,#24142,#24143);
#19418=AXIS2_PLACEMENT_3D('',#36608,#24144,#24145);
#19419=AXIS2_PLACEMENT_3D('',#36610,#24146,#24147);
#19420=AXIS2_PLACEMENT_3D('',#36612,#24149,#24150);
#19421=AXIS2_PLACEMENT_3D('',#36618,#24154,#24155);
#19422=AXIS2_PLACEMENT_3D('',#36624,#24159,#24160);
#19423=AXIS2_PLACEMENT_3D('',#36630,#24164,#24165);
#19424=AXIS2_PLACEMENT_3D('',#36631,#24166,#24167);
#19425=AXIS2_PLACEMENT_3D('',#36632,#24168,#24169);
#19426=AXIS2_PLACEMENT_3D('',#36633,#24170,#24171);
#19427=AXIS2_PLACEMENT_3D('',#36634,#24172,#24173);
#19428=AXIS2_PLACEMENT_3D('',#36635,#24174,#24175);
#19429=AXIS2_PLACEMENT_3D('',#36636,#24176,#24177);
#19430=AXIS2_PLACEMENT_3D('',#36637,#24178,#24179);
#19431=AXIS2_PLACEMENT_3D('',#36638,#24180,#24181);
#19432=AXIS2_PLACEMENT_3D('',#36639,#24182,#24183);
#19433=AXIS2_PLACEMENT_3D('',#36640,#24184,#24185);
#19434=AXIS2_PLACEMENT_3D('',#36641,#24186,#24187);
#19435=AXIS2_PLACEMENT_3D('',#36642,#24188,#24189);
#19436=AXIS2_PLACEMENT_3D('',#36643,#24190,#24191);
#19437=AXIS2_PLACEMENT_3D('',#36644,#24192,#24193);
#19438=DIRECTION('axis',(0.,0.,1.));
#19439=DIRECTION('refdir',(1.,0.,0.));
#19440=DIRECTION('axis',(0.,0.,1.));
#19441=DIRECTION('refdir',(1.,0.,0.));
#19442=DIRECTION('center_axis',(-1.E-14,-1.,0.));
#19443=DIRECTION('ref_axis',(1.,-1.E-14,1.E-14));
#19444=DIRECTION('',(0.,0.,-1.));
#19445=DIRECTION('',(1.,-1.E-14,1.E-14));
#19446=DIRECTION('',(-1.E-14,0.,1.));
#19447=DIRECTION('',(1.,-1.E-14,1.E-14));
#19448=DIRECTION('center_axis',(-1.E-14,-1.,0.));
#19449=DIRECTION('ref_axis',(1.,-1.E-14,0.));
#19450=DIRECTION('center_axis',(-1.E-14,-1.,0.));
#19451=DIRECTION('ref_axis',(1.,-1.E-14,0.));
#19452=DIRECTION('center_axis',(-1.E-14,-1.,0.));
#19453=DIRECTION('ref_axis',(1.,-1.E-14,0.));
#19454=DIRECTION('center_axis',(-1.E-14,-1.,0.));
#19455=DIRECTION('ref_axis',(1.,-1.E-14,0.));
#19456=DIRECTION('center_axis',(-1.E-14,-1.,0.));
#19457=DIRECTION('ref_axis',(1.,-1.E-14,0.));
#19458=DIRECTION('center_axis',(-1.E-14,-1.,0.));
#19459=DIRECTION('ref_axis',(1.,-1.E-14,0.));
#19460=DIRECTION('center_axis',(-1.E-14,-1.,0.));
#19461=DIRECTION('ref_axis',(1.,-1.E-14,0.));
#19462=DIRECTION('center_axis',(-1.E-14,-1.,0.));
#19463=DIRECTION('ref_axis',(1.,-1.E-14,0.));
#19464=DIRECTION('center_axis',(-1.E-14,-1.,0.));
#19465=DIRECTION('ref_axis',(1.,-1.E-14,0.));
#19466=DIRECTION('center_axis',(-1.E-14,-1.,0.));
#19467=DIRECTION('ref_axis',(1.,-1.E-14,0.));
#19468=DIRECTION('center_axis',(-1.E-14,-1.,0.));
#19469=DIRECTION('ref_axis',(1.,-1.E-14,0.));
#19470=DIRECTION('center_axis',(-1.E-14,-1.,0.));
#19471=DIRECTION('ref_axis',(1.,-1.E-14,0.));
#19472=DIRECTION('center_axis',(-1.E-14,-1.,0.));
#19473=DIRECTION('ref_axis',(1.,-1.E-14,0.));
#19474=DIRECTION('center_axis',(-1.E-14,-1.,0.));
#19475=DIRECTION('ref_axis',(1.,-1.E-14,0.));
#19476=DIRECTION('center_axis',(-1.E-14,-1.,0.));
#19477=DIRECTION('ref_axis',(1.,-1.E-14,0.));
#19478=DIRECTION('center_axis',(-1.E-14,-1.,0.));
#19479=DIRECTION('ref_axis',(1.,-1.E-14,0.));
#19480=DIRECTION('center_axis',(-1.E-14,-1.,0.));
#19481=DIRECTION('ref_axis',(1.,-1.E-14,0.));
#19482=DIRECTION('center_axis',(-1.E-14,-1.,0.));
#19483=DIRECTION('ref_axis',(1.,-1.E-14,0.));
#19484=DIRECTION('center_axis',(-1.E-14,-1.,0.));
#19485=DIRECTION('ref_axis',(1.,-1.E-14,0.));
#19486=DIRECTION('center_axis',(-1.E-14,-1.,0.));
#19487=DIRECTION('ref_axis',(1.,-1.E-14,0.));
#19488=DIRECTION('center_axis',(-1.E-14,-1.,0.));
#19489=DIRECTION('ref_axis',(1.,-1.E-14,0.));
#19490=DIRECTION('center_axis',(-1.E-14,-1.,0.));
#19491=DIRECTION('ref_axis',(1.,-1.E-14,0.));
#19492=DIRECTION('center_axis',(-1.E-14,-1.,0.));
#19493=DIRECTION('ref_axis',(1.,-1.E-14,0.));
#19494=DIRECTION('center_axis',(-1.E-14,-1.,0.));
#19495=DIRECTION('ref_axis',(1.,-1.E-14,0.));
#19496=DIRECTION('center_axis',(-1.E-14,-1.,0.));
#19497=DIRECTION('ref_axis',(1.,-1.E-14,0.));
#19498=DIRECTION('center_axis',(-1.E-14,-1.,0.));
#19499=DIRECTION('ref_axis',(1.,-1.E-14,0.));
#19500=DIRECTION('',(1.,-1.E-14,1.E-14));
#19501=DIRECTION('',(-1.E-14,0.,1.));
#19502=DIRECTION('',(1.,-1.E-14,9.60574466455073E-15));
#19503=DIRECTION('',(-1.E-14,0.,1.));
#19504=DIRECTION('',(1.,-1.E-14,1.E-14));
#19505=DIRECTION('',(-1.1020425574104E-14,1.020425574104E-29,1.));
#19506=DIRECTION('',(1.,-1.E-14,9.60574466455073E-15));
#19507=DIRECTION('',(-1.E-14,0.,1.));
#19508=DIRECTION('',(1.,-1.E-14,1.E-14));
#19509=DIRECTION('',(-1.1020425574104E-14,1.020425574104E-29,1.));
#19510=DIRECTION('',(1.,-1.E-14,9.60574466455073E-15));
#19511=DIRECTION('',(-1.E-14,0.,1.));
#19512=DIRECTION('',(1.,-1.E-14,1.E-14));
#19513=DIRECTION('',(-1.E-14,0.,1.));
#19514=DIRECTION('',(1.,-1.E-14,9.60574466455073E-15));
#19515=DIRECTION('',(-1.E-14,0.,1.));
#19516=DIRECTION('',(1.,-1.E-14,1.E-14));
#19517=DIRECTION('',(-1.E-14,0.,1.));
#19518=DIRECTION('',(1.,-1.E-14,9.60574466455073E-15));
#19519=DIRECTION('',(-1.E-14,0.,1.));
#19520=DIRECTION('',(1.,-1.E-14,1.E-14));
#19521=DIRECTION('',(-1.E-14,0.,1.));
#19522=DIRECTION('',(1.,-1.E-14,9.60574466455073E-15));
#19523=DIRECTION('',(-1.E-14,0.,1.));
#19524=DIRECTION('',(1.,-1.E-14,1.E-14));
#19525=DIRECTION('',(-1.E-14,0.,1.));
#19526=DIRECTION('',(1.,-1.E-14,9.60574466455073E-15));
#19527=DIRECTION('',(-1.E-14,0.,1.));
#19528=DIRECTION('',(1.,-1.E-14,1.E-14));
#19529=DIRECTION('',(-1.E-14,0.,1.));
#19530=DIRECTION('',(1.,-1.E-14,9.60574466455073E-15));
#19531=DIRECTION('',(-1.E-14,0.,1.));
#19532=DIRECTION('',(1.,-1.E-14,1.E-14));
#19533=DIRECTION('',(-1.E-14,0.,1.));
#19534=DIRECTION('',(1.,-1.E-14,9.60574466455073E-15));
#19535=DIRECTION('',(-1.E-14,0.,1.));
#19536=DIRECTION('',(1.,-1.E-14,1.E-14));
#19537=DIRECTION('',(-1.E-14,0.,1.));
#19538=DIRECTION('',(1.,-1.E-14,9.60574466455073E-15));
#19539=DIRECTION('',(-1.E-14,0.,1.));
#19540=DIRECTION('',(1.,-1.E-14,1.E-14));
#19541=DIRECTION('',(-1.E-14,0.,1.));
#19542=DIRECTION('',(1.,-1.E-14,9.60574466455073E-15));
#19543=DIRECTION('',(-1.E-14,0.,1.));
#19544=DIRECTION('',(1.,-1.E-14,1.E-14));
#19545=DIRECTION('',(-1.E-14,0.,1.));
#19546=DIRECTION('',(1.,-1.E-14,9.60574466455073E-15));
#19547=DIRECTION('',(-1.E-14,0.,1.));
#19548=DIRECTION('',(1.,-1.E-14,1.E-14));
#19549=DIRECTION('',(-1.E-14,0.,1.));
#19550=DIRECTION('',(1.,-1.E-14,9.60574466455073E-15));
#19551=DIRECTION('',(-1.E-14,0.,1.));
#19552=DIRECTION('',(1.,-1.E-14,1.E-14));
#19553=DIRECTION('',(-1.E-14,0.,1.));
#19554=DIRECTION('',(1.,-1.E-14,9.60574466455073E-15));
#19555=DIRECTION('',(-1.E-14,0.,1.));
#19556=DIRECTION('',(1.,-1.E-14,1.E-14));
#19557=DIRECTION('',(-1.E-14,0.,1.));
#19558=DIRECTION('',(1.,-1.E-14,9.60574466455073E-15));
#19559=DIRECTION('',(-1.E-14,0.,1.));
#19560=DIRECTION('',(1.,-1.E-14,1.E-14));
#19561=DIRECTION('',(-1.E-14,0.,1.));
#19562=DIRECTION('',(1.,-1.E-14,9.60574466455073E-15));
#19563=DIRECTION('',(-1.E-14,0.,1.));
#19564=DIRECTION('',(1.,-1.E-14,1.E-14));
#19565=DIRECTION('',(-1.E-14,0.,1.));
#19566=DIRECTION('',(1.,-1.E-14,9.60574466455073E-15));
#19567=DIRECTION('',(-1.E-14,0.,1.));
#19568=DIRECTION('',(1.,-1.E-14,1.E-14));
#19569=DIRECTION('',(-1.E-14,0.,1.));
#19570=DIRECTION('',(1.,-1.E-14,9.60574466455073E-15));
#19571=DIRECTION('',(-1.E-14,0.,1.));
#19572=DIRECTION('',(1.,-1.E-14,1.E-14));
#19573=DIRECTION('',(-1.E-14,0.,1.));
#19574=DIRECTION('',(1.,-1.E-14,9.60574466455073E-15));
#19575=DIRECTION('',(-1.E-14,0.,1.));
#19576=DIRECTION('',(1.,-1.E-14,1.E-14));
#19577=DIRECTION('',(-1.E-14,0.,1.));
#19578=DIRECTION('',(1.,-1.E-14,9.60574466455073E-15));
#19579=DIRECTION('',(-1.E-14,0.,1.));
#19580=DIRECTION('',(1.,-1.E-14,1.E-14));
#19581=DIRECTION('',(-1.E-14,0.,1.));
#19582=DIRECTION('',(1.,-1.E-14,9.60574466455073E-15));
#19583=DIRECTION('',(-1.E-14,0.,1.));
#19584=DIRECTION('',(1.,-1.E-14,1.E-14));
#19585=DIRECTION('',(-1.E-14,0.,1.));
#19586=DIRECTION('',(1.,-1.E-14,9.60574466455073E-15));
#19587=DIRECTION('',(-1.E-14,0.,1.));
#19588=DIRECTION('',(1.,-1.E-14,1.E-14));
#19589=DIRECTION('',(-1.E-14,0.,1.));
#19590=DIRECTION('',(1.,-1.E-14,9.60574466455073E-15));
#19591=DIRECTION('',(-1.E-14,0.,1.));
#19592=DIRECTION('',(1.,-1.E-14,1.E-14));
#19593=DIRECTION('',(-1.E-14,0.,1.));
#19594=DIRECTION('',(1.,-1.E-14,9.60574466455073E-15));
#19595=DIRECTION('',(-1.E-14,0.,1.));
#19596=DIRECTION('',(1.,-1.E-14,1.E-14));
#19597=DIRECTION('',(-1.E-14,0.,1.));
#19598=DIRECTION('',(1.,-1.E-14,9.60574466455073E-15));
#19599=DIRECTION('',(-1.E-14,0.,1.));
#19600=DIRECTION('',(1.,-1.E-14,1.E-14));
#19601=DIRECTION('',(-1.E-14,0.,1.));
#19602=DIRECTION('',(1.,-1.E-14,9.60574466455073E-15));
#19603=DIRECTION('',(-1.E-14,0.,1.));
#19604=DIRECTION('center_axis',(-1.E-14,-1.,0.));
#19605=DIRECTION('ref_axis',(1.,-1.E-14,1.E-14));
#19606=DIRECTION('',(0.,0.,1.));
#19607=DIRECTION('',(1.,-1.E-14,1.E-14));
#19608=DIRECTION('',(-1.E-14,0.,1.));
#19609=DIRECTION('',(1.,-1.E-14,1.E-14));
#19610=DIRECTION('',(1.,-1.E-14,1.E-14));
#19611=DIRECTION('',(-1.E-14,0.,1.));
#19612=DIRECTION('',(1.,-1.E-14,9.60574466455073E-15));
#19613=DIRECTION('',(-1.E-14,0.,1.));
#19614=DIRECTION('',(1.,-1.E-14,1.E-14));
#19615=DIRECTION('',(-1.E-14,0.,1.));
#19616=DIRECTION('',(1.,-1.E-14,9.60574466455073E-15));
#19617=DIRECTION('',(-1.E-14,0.,1.));
#19618=DIRECTION('',(1.,-1.E-14,1.E-14));
#19619=DIRECTION('',(-1.E-14,0.,1.));
#19620=DIRECTION('',(1.,-1.E-14,9.60574466455073E-15));
#19621=DIRECTION('',(-1.E-14,0.,1.));
#19622=DIRECTION('',(1.,-1.E-14,1.E-14));
#19623=DIRECTION('',(-1.E-14,0.,1.));
#19624=DIRECTION('',(1.,-1.E-14,9.60574466455073E-15));
#19625=DIRECTION('',(-1.E-14,0.,1.));
#19626=DIRECTION('',(1.,-1.E-14,1.E-14));
#19627=DIRECTION('',(-1.E-14,0.,1.));
#19628=DIRECTION('',(1.,-1.E-14,9.60574466455073E-15));
#19629=DIRECTION('',(-1.E-14,0.,1.));
#19630=DIRECTION('',(1.,-1.E-14,1.E-14));
#19631=DIRECTION('',(-1.E-14,0.,1.));
#19632=DIRECTION('',(1.,-1.E-14,9.60574466455073E-15));
#19633=DIRECTION('',(-1.E-14,0.,1.));
#19634=DIRECTION('',(1.,-1.E-14,1.E-14));
#19635=DIRECTION('',(-1.E-14,0.,1.));
#19636=DIRECTION('',(1.,-1.E-14,9.60574466455073E-15));
#19637=DIRECTION('',(-1.E-14,0.,1.));
#19638=DIRECTION('',(1.,-1.E-14,1.E-14));
#19639=DIRECTION('',(-1.E-14,0.,1.));
#19640=DIRECTION('',(1.,-1.E-14,9.60574466455073E-15));
#19641=DIRECTION('',(-1.E-14,0.,1.));
#19642=DIRECTION('',(1.,-1.E-14,1.E-14));
#19643=DIRECTION('',(-1.E-14,0.,1.));
#19644=DIRECTION('',(1.,-1.E-14,9.60574466455073E-15));
#19645=DIRECTION('',(-1.E-14,0.,1.));
#19646=DIRECTION('',(1.,-1.E-14,1.E-14));
#19647=DIRECTION('',(-1.E-14,0.,1.));
#19648=DIRECTION('',(1.,-1.E-14,9.60574466455073E-15));
#19649=DIRECTION('',(-1.E-14,0.,1.));
#19650=DIRECTION('',(1.,-1.E-14,1.E-14));
#19651=DIRECTION('',(-1.E-14,0.,1.));
#19652=DIRECTION('',(1.,-1.E-14,9.60574466455073E-15));
#19653=DIRECTION('',(-1.E-14,0.,1.));
#19654=DIRECTION('',(1.,-1.E-14,1.E-14));
#19655=DIRECTION('',(-1.E-14,0.,1.));
#19656=DIRECTION('',(1.,-1.E-14,9.60574466455073E-15));
#19657=DIRECTION('',(-1.E-14,0.,1.));
#19658=DIRECTION('',(1.,-1.E-14,1.E-14));
#19659=DIRECTION('',(-1.E-14,0.,1.));
#19660=DIRECTION('',(1.,-1.E-14,9.60574466455073E-15));
#19661=DIRECTION('',(-1.E-14,0.,1.));
#19662=DIRECTION('',(1.,-1.E-14,1.E-14));
#19663=DIRECTION('',(-1.E-14,0.,1.));
#19664=DIRECTION('',(1.,-1.E-14,9.60574466455073E-15));
#19665=DIRECTION('',(-1.E-14,0.,1.));
#19666=DIRECTION('',(1.,-1.E-14,1.E-14));
#19667=DIRECTION('',(-1.E-14,0.,1.));
#19668=DIRECTION('',(1.,-1.E-14,9.60574466455073E-15));
#19669=DIRECTION('',(-1.E-14,0.,1.));
#19670=DIRECTION('',(1.,-1.E-14,1.E-14));
#19671=DIRECTION('',(-1.E-14,0.,1.));
#19672=DIRECTION('',(1.,-1.E-14,9.60574466455073E-15));
#19673=DIRECTION('',(-1.E-14,0.,1.));
#19674=DIRECTION('',(1.,-1.E-14,1.E-14));
#19675=DIRECTION('',(-1.E-14,0.,1.));
#19676=DIRECTION('',(1.,-1.E-14,9.60574466455073E-15));
#19677=DIRECTION('',(-1.E-14,0.,1.));
#19678=DIRECTION('',(1.,-1.E-14,1.E-14));
#19679=DIRECTION('',(-1.E-14,0.,1.));
#19680=DIRECTION('',(1.,-1.E-14,9.60574466455073E-15));
#19681=DIRECTION('',(-1.E-14,0.,1.));
#19682=DIRECTION('',(1.,-1.E-14,1.E-14));
#19683=DIRECTION('',(-1.E-14,0.,1.));
#19684=DIRECTION('',(1.,-1.E-14,9.60574466455073E-15));
#19685=DIRECTION('',(-1.E-14,0.,1.));
#19686=DIRECTION('',(1.,-1.E-14,1.E-14));
#19687=DIRECTION('',(-1.E-14,0.,1.));
#19688=DIRECTION('',(1.,-1.E-14,9.60574466455073E-15));
#19689=DIRECTION('',(-1.E-14,0.,1.));
#19690=DIRECTION('',(1.,-1.E-14,1.E-14));
#19691=DIRECTION('',(-1.E-14,0.,1.));
#19692=DIRECTION('',(1.,-1.E-14,9.60574466455073E-15));
#19693=DIRECTION('',(-1.E-14,0.,1.));
#19694=DIRECTION('',(1.,-1.E-14,1.E-14));
#19695=DIRECTION('',(-1.E-14,0.,1.));
#19696=DIRECTION('',(1.,-1.E-14,9.60574466455073E-15));
#19697=DIRECTION('',(-1.E-14,0.,1.));
#19698=DIRECTION('',(1.,-1.E-14,1.E-14));
#19699=DIRECTION('',(-1.E-14,0.,1.));
#19700=DIRECTION('',(1.,-1.E-14,9.60574466455073E-15));
#19701=DIRECTION('',(-1.E-14,0.,1.));
#19702=DIRECTION('',(1.,-1.E-14,1.E-14));
#19703=DIRECTION('',(-1.E-14,0.,1.));
#19704=DIRECTION('',(1.,-1.E-14,9.60574466455073E-15));
#19705=DIRECTION('',(-1.1020425574104E-14,1.020425574104E-29,1.));
#19706=DIRECTION('',(1.,-1.E-14,1.E-14));
#19707=DIRECTION('',(-1.E-14,0.,1.));
#19708=DIRECTION('',(1.,-1.E-14,9.60574466455073E-15));
#19709=DIRECTION('',(-1.1020425574104E-14,1.020425574104E-29,1.));
#19710=DIRECTION('',(1.,-1.E-14,1.E-14));
#19711=DIRECTION('',(-1.E-14,0.,1.));
#19712=DIRECTION('',(1.,-1.E-14,9.60574466455073E-15));
#19713=DIRECTION('',(-1.E-14,0.,1.));
#19714=DIRECTION('center_axis',(-1.E-14,-1.,0.));
#19715=DIRECTION('ref_axis',(1.,-1.E-14,0.));
#19716=DIRECTION('center_axis',(-1.E-14,-1.,0.));
#19717=DIRECTION('ref_axis',(1.,-1.E-14,0.));
#19718=DIRECTION('center_axis',(-1.E-14,-1.,0.));
#19719=DIRECTION('ref_axis',(1.,-1.E-14,0.));
#19720=DIRECTION('center_axis',(-1.E-14,-1.,0.));
#19721=DIRECTION('ref_axis',(1.,-1.E-14,0.));
#19722=DIRECTION('center_axis',(-1.E-14,-1.,0.));
#19723=DIRECTION('ref_axis',(1.,-1.E-14,0.));
#19724=DIRECTION('center_axis',(-1.E-14,-1.,0.));
#19725=DIRECTION('ref_axis',(1.,-1.E-14,0.));
#19726=DIRECTION('center_axis',(-1.E-14,-1.,0.));
#19727=DIRECTION('ref_axis',(1.,-1.E-14,0.));
#19728=DIRECTION('center_axis',(-1.E-14,-1.,0.));
#19729=DIRECTION('ref_axis',(1.,-1.E-14,0.));
#19730=DIRECTION('center_axis',(-1.E-14,-1.,0.));
#19731=DIRECTION('ref_axis',(1.,-1.E-14,0.));
#19732=DIRECTION('center_axis',(-1.E-14,-1.,0.));
#19733=DIRECTION('ref_axis',(1.,-1.E-14,0.));
#19734=DIRECTION('center_axis',(-1.E-14,-1.,0.));
#19735=DIRECTION('ref_axis',(1.,-1.E-14,0.));
#19736=DIRECTION('center_axis',(-1.E-14,-1.,0.));
#19737=DIRECTION('ref_axis',(1.,-1.E-14,0.));
#19738=DIRECTION('center_axis',(-1.E-14,-1.,0.));
#19739=DIRECTION('ref_axis',(1.,-1.E-14,0.));
#19740=DIRECTION('center_axis',(-1.E-14,-1.,0.));
#19741=DIRECTION('ref_axis',(1.,-1.E-14,0.));
#19742=DIRECTION('center_axis',(-1.E-14,-1.,0.));
#19743=DIRECTION('ref_axis',(1.,-1.E-14,0.));
#19744=DIRECTION('center_axis',(-1.E-14,-1.,0.));
#19745=DIRECTION('ref_axis',(1.,-1.E-14,0.));
#19746=DIRECTION('center_axis',(-1.E-14,-1.,0.));
#19747=DIRECTION('ref_axis',(1.,-1.E-14,0.));
#19748=DIRECTION('center_axis',(-1.E-14,-1.,0.));
#19749=DIRECTION('ref_axis',(1.,-1.E-14,0.));
#19750=DIRECTION('center_axis',(-1.E-14,-1.,0.));
#19751=DIRECTION('ref_axis',(1.,-1.E-14,0.));
#19752=DIRECTION('center_axis',(-1.E-14,-1.,0.));
#19753=DIRECTION('ref_axis',(1.,-1.E-14,0.));
#19754=DIRECTION('center_axis',(-1.E-14,-1.,0.));
#19755=DIRECTION('ref_axis',(1.,-1.E-14,0.));
#19756=DIRECTION('center_axis',(-1.E-14,-1.,0.));
#19757=DIRECTION('ref_axis',(1.,-1.E-14,0.));
#19758=DIRECTION('center_axis',(-1.E-14,-1.,0.));
#19759=DIRECTION('ref_axis',(1.,-1.E-14,0.));
#19760=DIRECTION('center_axis',(-1.E-14,-1.,0.));
#19761=DIRECTION('ref_axis',(1.,-1.E-14,0.));
#19762=DIRECTION('center_axis',(-1.E-14,-1.,0.));
#19763=DIRECTION('ref_axis',(1.,-1.E-14,0.));
#19764=DIRECTION('center_axis',(-1.E-14,-1.,0.));
#19765=DIRECTION('ref_axis',(1.,-1.E-14,0.));
#19766=DIRECTION('center_axis',(-1.,1.E-14,-1.E-14));
#19767=DIRECTION('ref_axis',(-1.E-14,-1.,-2.64060752475192E-45));
#19768=DIRECTION('',(1.E-14,1.,0.));
#19769=DIRECTION('',(1.E-14,1.,0.));
#19770=DIRECTION('center_axis',(1.E-14,1.,0.));
#19771=DIRECTION('ref_axis',(-1.,1.E-14,0.));
#19772=DIRECTION('',(1.E-14,1.,0.));
#19773=DIRECTION('center_axis',(1.E-14,1.,0.));
#19774=DIRECTION('ref_axis',(-1.,1.E-14,0.));
#19775=DIRECTION('',(1.E-14,1.,0.));
#19776=DIRECTION('center_axis',(1.E-14,1.,0.));
#19777=DIRECTION('ref_axis',(-1.,1.E-14,0.));
#19778=DIRECTION('',(1.E-14,1.,0.));
#19779=DIRECTION('center_axis',(1.E-14,1.,0.));
#19780=DIRECTION('ref_axis',(-1.,1.E-14,0.));
#19781=DIRECTION('',(1.E-14,1.,0.));
#19782=DIRECTION('center_axis',(1.E-14,1.,0.));
#19783=DIRECTION('ref_axis',(-1.,1.E-14,0.));
#19784=DIRECTION('',(1.E-14,1.,0.));
#19785=DIRECTION('center_axis',(1.E-14,1.,0.));
#19786=DIRECTION('ref_axis',(-1.,1.E-14,0.));
#19787=DIRECTION('',(1.E-14,1.,0.));
#19788=DIRECTION('center_axis',(1.E-14,1.,0.));
#19789=DIRECTION('ref_axis',(-1.,1.E-14,0.));
#19790=DIRECTION('',(1.E-14,1.,0.));
#19791=DIRECTION('center_axis',(1.E-14,1.,0.));
#19792=DIRECTION('ref_axis',(-1.,1.E-14,0.));
#19793=DIRECTION('',(1.E-14,1.,0.));
#19794=DIRECTION('center_axis',(1.E-14,1.,0.));
#19795=DIRECTION('ref_axis',(-1.,1.E-14,0.));
#19796=DIRECTION('',(1.E-14,1.,0.));
#19797=DIRECTION('center_axis',(1.E-14,1.,0.));
#19798=DIRECTION('ref_axis',(-1.,1.E-14,0.));
#19799=DIRECTION('',(1.E-14,1.,0.));
#19800=DIRECTION('center_axis',(1.E-14,1.,0.));
#19801=DIRECTION('ref_axis',(-1.,1.E-14,0.));
#19802=DIRECTION('',(1.E-14,1.,0.));
#19803=DIRECTION('center_axis',(1.E-14,1.,0.));
#19804=DIRECTION('ref_axis',(-1.,1.E-14,0.));
#19805=DIRECTION('',(1.E-14,1.,0.));
#19806=DIRECTION('center_axis',(1.E-14,1.,0.));
#19807=DIRECTION('ref_axis',(-1.,1.E-14,0.));
#19808=DIRECTION('',(1.E-14,1.,0.));
#19809=DIRECTION('center_axis',(1.E-14,1.,0.));
#19810=DIRECTION('ref_axis',(-1.,1.E-14,0.));
#19811=DIRECTION('',(1.E-14,1.,0.));
#19812=DIRECTION('center_axis',(1.E-14,1.,0.));
#19813=DIRECTION('ref_axis',(-1.,1.E-14,0.));
#19814=DIRECTION('',(1.E-14,1.,0.));
#19815=DIRECTION('center_axis',(1.E-14,1.,0.));
#19816=DIRECTION('ref_axis',(-1.,1.E-14,0.));
#19817=DIRECTION('',(1.E-14,1.,0.));
#19818=DIRECTION('center_axis',(1.E-14,1.,0.));
#19819=DIRECTION('ref_axis',(-1.,1.E-14,0.));
#19820=DIRECTION('',(1.E-14,1.,0.));
#19821=DIRECTION('center_axis',(1.E-14,1.,0.));
#19822=DIRECTION('ref_axis',(-1.,1.E-14,0.));
#19823=DIRECTION('',(1.E-14,1.,0.));
#19824=DIRECTION('center_axis',(1.E-14,1.,0.));
#19825=DIRECTION('ref_axis',(-1.,1.E-14,0.));
#19826=DIRECTION('',(1.E-14,1.,0.));
#19827=DIRECTION('center_axis',(1.E-14,1.,0.));
#19828=DIRECTION('ref_axis',(-1.,1.E-14,0.));
#19829=DIRECTION('',(1.E-14,1.,0.));
#19830=DIRECTION('center_axis',(1.E-14,1.,0.));
#19831=DIRECTION('ref_axis',(-1.,1.E-14,0.));
#19832=DIRECTION('',(1.E-14,1.,0.));
#19833=DIRECTION('center_axis',(1.E-14,1.,0.));
#19834=DIRECTION('ref_axis',(-1.,1.E-14,0.));
#19835=DIRECTION('',(1.E-14,1.,0.));
#19836=DIRECTION('center_axis',(1.E-14,1.,0.));
#19837=DIRECTION('ref_axis',(-1.,1.E-14,0.));
#19838=DIRECTION('',(1.E-14,1.,0.));
#19839=DIRECTION('center_axis',(1.E-14,1.,0.));
#19840=DIRECTION('ref_axis',(-1.,1.E-14,0.));
#19841=DIRECTION('',(1.E-14,1.,0.));
#19842=DIRECTION('center_axis',(1.E-14,1.,0.));
#19843=DIRECTION('ref_axis',(-1.,1.E-14,0.));
#19844=DIRECTION('',(1.E-14,1.,0.));
#19845=DIRECTION('center_axis',(1.E-14,1.,0.));
#19846=DIRECTION('ref_axis',(-1.,1.E-14,0.));
#19847=DIRECTION('',(1.E-14,1.,0.));
#19848=DIRECTION('center_axis',(-1.,1.E-14,-1.E-14));
#19849=DIRECTION('ref_axis',(-1.E-14,-1.,-2.64060752475192E-45));
#19850=DIRECTION('',(1.E-14,1.,0.));
#19851=DIRECTION('',(1.E-14,1.,0.));
#19852=DIRECTION('center_axis',(-1.,1.E-14,-1.1020425574104E-14));
#19853=DIRECTION('ref_axis',(-1.1020425574104E-14,1.020425574104E-29,1.));
#19854=DIRECTION('',(1.E-14,1.,0.));
#19855=DIRECTION('',(1.E-14,1.,0.));
#19856=DIRECTION('center_axis',(-1.,1.E-14,-1.1020425574104E-14));
#19857=DIRECTION('ref_axis',(-1.1020425574104E-14,1.020425574104E-29,1.));
#19858=DIRECTION('',(1.E-14,1.,0.));
#19859=DIRECTION('',(1.E-14,1.,0.));
#19860=DIRECTION('center_axis',(-1.,1.E-14,-1.E-14));
#19861=DIRECTION('ref_axis',(-1.E-14,-1.,-2.64060752475192E-45));
#19862=DIRECTION('',(1.E-14,1.,0.));
#19863=DIRECTION('',(1.E-14,1.,0.));
#19864=DIRECTION('center_axis',(-1.,1.E-14,-1.E-14));
#19865=DIRECTION('ref_axis',(-1.E-14,-1.,-2.64060752475192E-45));
#19866=DIRECTION('',(1.E-14,1.,0.));
#19867=DIRECTION('',(1.E-14,1.,0.));
#19868=DIRECTION('center_axis',(-1.,1.E-14,-1.E-14));
#19869=DIRECTION('ref_axis',(-1.E-14,-1.,-2.64060752475192E-45));
#19870=DIRECTION('',(1.E-14,1.,0.));
#19871=DIRECTION('',(1.E-14,1.,0.));
#19872=DIRECTION('center_axis',(-1.,1.E-14,-1.E-14));
#19873=DIRECTION('ref_axis',(-1.E-14,-1.,-2.64060752475192E-45));
#19874=DIRECTION('',(1.E-14,1.,0.));
#19875=DIRECTION('',(1.E-14,1.,0.));
#19876=DIRECTION('center_axis',(-1.,1.E-14,-1.E-14));
#19877=DIRECTION('ref_axis',(-1.E-14,-1.,-2.64060752475192E-45));
#19878=DIRECTION('',(1.E-14,1.,0.));
#19879=DIRECTION('',(1.E-14,1.,0.));
#19880=DIRECTION('center_axis',(-1.,1.E-14,-1.E-14));
#19881=DIRECTION('ref_axis',(-1.E-14,-1.,-2.64060752475192E-45));
#19882=DIRECTION('',(1.E-14,1.,0.));
#19883=DIRECTION('',(1.E-14,1.,0.));
#19884=DIRECTION('center_axis',(-1.,1.E-14,-1.E-14));
#19885=DIRECTION('ref_axis',(-1.E-14,-1.,-2.64060752475192E-45));
#19886=DIRECTION('',(1.E-14,1.,0.));
#19887=DIRECTION('',(1.E-14,1.,0.));
#19888=DIRECTION('center_axis',(-1.,1.E-14,-1.E-14));
#19889=DIRECTION('ref_axis',(-1.E-14,-1.,-2.64060752475192E-45));
#19890=DIRECTION('',(1.E-14,1.,0.));
#19891=DIRECTION('',(1.E-14,1.,0.));
#19892=DIRECTION('center_axis',(-1.,1.E-14,-1.E-14));
#19893=DIRECTION('ref_axis',(-1.E-14,-1.,-2.64060752475192E-45));
#19894=DIRECTION('',(1.E-14,1.,0.));
#19895=DIRECTION('',(1.E-14,1.,0.));
#19896=DIRECTION('center_axis',(-1.,1.E-14,-1.E-14));
#19897=DIRECTION('ref_axis',(-1.E-14,-1.,-2.64060752475192E-45));
#19898=DIRECTION('',(1.E-14,1.,0.));
#19899=DIRECTION('',(1.E-14,1.,0.));
#19900=DIRECTION('center_axis',(-1.,1.E-14,-1.E-14));
#19901=DIRECTION('ref_axis',(-1.E-14,-1.,-2.64060752475192E-45));
#19902=DIRECTION('',(1.E-14,1.,0.));
#19903=DIRECTION('',(1.E-14,1.,0.));
#19904=DIRECTION('center_axis',(-1.,1.E-14,-1.E-14));
#19905=DIRECTION('ref_axis',(-1.E-14,-1.,-2.64060752475192E-45));
#19906=DIRECTION('',(1.E-14,1.,0.));
#19907=DIRECTION('',(1.E-14,1.,0.));
#19908=DIRECTION('center_axis',(-1.,1.E-14,-1.E-14));
#19909=DIRECTION('ref_axis',(-1.E-14,-1.,-2.64060752475192E-45));
#19910=DIRECTION('',(1.E-14,1.,0.));
#19911=DIRECTION('',(1.E-14,1.,0.));
#19912=DIRECTION('center_axis',(-1.,1.E-14,-1.E-14));
#19913=DIRECTION('ref_axis',(-1.E-14,-1.,-2.64060752475192E-45));
#19914=DIRECTION('',(1.E-14,1.,0.));
#19915=DIRECTION('',(1.E-14,1.,0.));
#19916=DIRECTION('center_axis',(-1.,1.E-14,-1.E-14));
#19917=DIRECTION('ref_axis',(-1.E-14,-1.,-2.64060752475192E-45));
#19918=DIRECTION('',(1.E-14,1.,0.));
#19919=DIRECTION('',(1.E-14,1.,0.));
#19920=DIRECTION('center_axis',(-1.,1.E-14,-1.E-14));
#19921=DIRECTION('ref_axis',(-1.E-14,-1.,-2.64060752475192E-45));
#19922=DIRECTION('',(1.E-14,1.,0.));
#19923=DIRECTION('',(1.E-14,1.,0.));
#19924=DIRECTION('center_axis',(-1.,1.E-14,-1.E-14));
#19925=DIRECTION('ref_axis',(-1.E-14,-1.,-2.64060752475192E-45));
#19926=DIRECTION('',(1.E-14,1.,0.));
#19927=DIRECTION('',(1.E-14,1.,0.));
#19928=DIRECTION('center_axis',(-1.,1.E-14,-1.E-14));
#19929=DIRECTION('ref_axis',(-1.E-14,-1.,-2.64060752475192E-45));
#19930=DIRECTION('',(1.E-14,1.,0.));
#19931=DIRECTION('',(1.E-14,1.,0.));
#19932=DIRECTION('center_axis',(-1.,1.E-14,-1.E-14));
#19933=DIRECTION('ref_axis',(-1.E-14,-1.,-2.64060752475192E-45));
#19934=DIRECTION('',(1.E-14,1.,0.));
#19935=DIRECTION('',(1.E-14,1.,0.));
#19936=DIRECTION('center_axis',(-1.,1.E-14,-1.E-14));
#19937=DIRECTION('ref_axis',(-1.E-14,-1.,-2.64060752475192E-45));
#19938=DIRECTION('',(1.E-14,1.,0.));
#19939=DIRECTION('',(1.E-14,1.,0.));
#19940=DIRECTION('center_axis',(-1.,1.E-14,-1.E-14));
#19941=DIRECTION('ref_axis',(-1.E-14,-1.,-2.64060752475192E-45));
#19942=DIRECTION('',(1.E-14,1.,0.));
#19943=DIRECTION('',(1.E-14,1.,0.));
#19944=DIRECTION('center_axis',(-1.,1.E-14,-1.E-14));
#19945=DIRECTION('ref_axis',(-1.E-14,-1.,-2.64060752475192E-45));
#19946=DIRECTION('',(1.E-14,1.,0.));
#19947=DIRECTION('',(1.E-14,1.,0.));
#19948=DIRECTION('center_axis',(-1.E-14,0.,1.));
#19949=DIRECTION('ref_axis',(1.,-1.E-14,1.E-14));
#19950=DIRECTION('',(1.E-14,1.,1.E-28));
#19951=DIRECTION('',(1.E-14,1.,0.));
#19952=DIRECTION('center_axis',(-1.,1.E-14,-1.E-14));
#19953=DIRECTION('ref_axis',(-1.E-14,-1.,-2.64060752475192E-45));
#19954=DIRECTION('',(1.E-14,1.,0.));
#19955=DIRECTION('center_axis',(-1.E-14,0.,1.));
#19956=DIRECTION('ref_axis',(1.,-1.E-14,1.E-14));
#19957=DIRECTION('',(1.E-14,1.,1.E-28));
#19958=DIRECTION('center_axis',(-9.60574466455073E-15,-3.94255335449275E-30,
1.));
#19959=DIRECTION('ref_axis',(1.,-1.E-14,9.60574466455073E-15));
#19960=DIRECTION('',(1.E-14,1.,0.));
#19961=DIRECTION('center_axis',(-1.,1.E-14,-1.E-14));
#19962=DIRECTION('ref_axis',(-1.E-14,-1.,-2.64060752475192E-45));
#19963=DIRECTION('',(1.E-14,1.,0.));
#19964=DIRECTION('center_axis',(-1.E-14,0.,1.));
#19965=DIRECTION('ref_axis',(1.,-1.E-14,1.E-14));
#19966=DIRECTION('center_axis',(-9.60574466455072E-15,-3.94255335449275E-30,
1.));
#19967=DIRECTION('ref_axis',(1.,-1.E-14,9.60574466455072E-15));
#19968=DIRECTION('',(1.E-14,1.,0.));
#19969=DIRECTION('center_axis',(-1.,1.E-14,-1.E-14));
#19970=DIRECTION('ref_axis',(-1.E-14,-1.,-2.64060752475192E-45));
#19971=DIRECTION('',(1.E-14,1.,0.));
#19972=DIRECTION('center_axis',(-1.E-14,0.,1.));
#19973=DIRECTION('ref_axis',(1.,-1.E-14,1.E-14));
#19974=DIRECTION('center_axis',(-9.60574466455072E-15,-3.94255335449275E-30,
1.));
#19975=DIRECTION('ref_axis',(1.,-1.E-14,9.60574466455072E-15));
#19976=DIRECTION('',(1.E-14,1.,0.));
#19977=DIRECTION('center_axis',(-1.,1.E-14,-1.E-14));
#19978=DIRECTION('ref_axis',(-1.E-14,-1.,-2.64060752475192E-45));
#19979=DIRECTION('',(1.E-14,1.,0.));
#19980=DIRECTION('center_axis',(-1.E-14,0.,1.));
#19981=DIRECTION('ref_axis',(1.,-1.E-14,1.E-14));
#19982=DIRECTION('center_axis',(-9.60574466455073E-15,-3.94255335449275E-30,
1.));
#19983=DIRECTION('ref_axis',(1.,-1.E-14,9.60574466455073E-15));
#19984=DIRECTION('',(1.E-14,1.,0.));
#19985=DIRECTION('center_axis',(-1.,1.E-14,-1.E-14));
#19986=DIRECTION('ref_axis',(-1.E-14,-1.,-2.64060752475192E-45));
#19987=DIRECTION('',(1.E-14,1.,0.));
#19988=DIRECTION('center_axis',(-1.E-14,0.,1.));
#19989=DIRECTION('ref_axis',(1.,-1.E-14,1.E-14));
#19990=DIRECTION('center_axis',(-9.60574466455073E-15,-3.94255335449275E-30,
1.));
#19991=DIRECTION('ref_axis',(1.,-1.E-14,9.60574466455073E-15));
#19992=DIRECTION('',(1.E-14,1.,0.));
#19993=DIRECTION('center_axis',(-1.,1.E-14,-1.E-14));
#19994=DIRECTION('ref_axis',(-1.E-14,-1.,-2.64060752475192E-45));
#19995=DIRECTION('',(1.E-14,1.,0.));
#19996=DIRECTION('center_axis',(-1.E-14,0.,1.));
#19997=DIRECTION('ref_axis',(1.,-1.E-14,1.E-14));
#19998=DIRECTION('center_axis',(-9.60574466455073E-15,-3.94255335449275E-30,
1.));
#19999=DIRECTION('ref_axis',(1.,-1.E-14,9.60574466455073E-15));
#20000=DIRECTION('',(1.E-14,1.,0.));
#20001=DIRECTION('center_axis',(-1.,1.E-14,-1.E-14));
#20002=DIRECTION('ref_axis',(-1.E-14,-1.,-2.64060752475192E-45));
#20003=DIRECTION('',(1.E-14,1.,0.));
#20004=DIRECTION('center_axis',(-1.E-14,0.,1.));
#20005=DIRECTION('ref_axis',(1.,-1.E-14,1.E-14));
#20006=DIRECTION('center_axis',(-9.60574466455073E-15,-3.94255335449275E-30,
1.));
#20007=DIRECTION('ref_axis',(1.,-1.E-14,9.60574466455073E-15));
#20008=DIRECTION('',(1.E-14,1.,0.));
#20009=DIRECTION('center_axis',(-1.,1.E-14,-1.E-14));
#20010=DIRECTION('ref_axis',(-1.E-14,-1.,-2.64060752475192E-45));
#20011=DIRECTION('',(1.E-14,1.,0.));
#20012=DIRECTION('center_axis',(-1.E-14,0.,1.));
#20013=DIRECTION('ref_axis',(1.,-1.E-14,1.E-14));
#20014=DIRECTION('center_axis',(-9.60574466455073E-15,-3.94255335449275E-30,
1.));
#20015=DIRECTION('ref_axis',(1.,-1.E-14,9.60574466455073E-15));
#20016=DIRECTION('',(1.E-14,1.,0.));
#20017=DIRECTION('center_axis',(-1.,1.E-14,-1.E-14));
#20018=DIRECTION('ref_axis',(-1.E-14,-1.,-2.64060752475192E-45));
#20019=DIRECTION('',(1.E-14,1.,0.));
#20020=DIRECTION('center_axis',(-1.E-14,0.,1.));
#20021=DIRECTION('ref_axis',(1.,-1.E-14,1.E-14));
#20022=DIRECTION('center_axis',(-9.60574466455073E-15,-3.94255335449275E-30,
1.));
#20023=DIRECTION('ref_axis',(1.,-1.E-14,9.60574466455073E-15));
#20024=DIRECTION('',(1.E-14,1.,0.));
#20025=DIRECTION('center_axis',(-1.,1.E-14,-1.E-14));
#20026=DIRECTION('ref_axis',(-1.E-14,-1.,-2.64060752475192E-45));
#20027=DIRECTION('',(1.E-14,1.,0.));
#20028=DIRECTION('center_axis',(-1.E-14,0.,1.));
#20029=DIRECTION('ref_axis',(1.,-1.E-14,1.E-14));
#20030=DIRECTION('center_axis',(-9.60574466455073E-15,-3.94255335449275E-30,
1.));
#20031=DIRECTION('ref_axis',(1.,-1.E-14,9.60574466455073E-15));
#20032=DIRECTION('',(1.E-14,1.,0.));
#20033=DIRECTION('center_axis',(-1.,1.E-14,-1.E-14));
#20034=DIRECTION('ref_axis',(-1.E-14,-1.,-2.64060752475192E-45));
#20035=DIRECTION('',(1.E-14,1.,0.));
#20036=DIRECTION('center_axis',(-1.E-14,0.,1.));
#20037=DIRECTION('ref_axis',(1.,-1.E-14,1.E-14));
#20038=DIRECTION('center_axis',(-9.60574466455073E-15,-3.94255335449275E-30,
1.));
#20039=DIRECTION('ref_axis',(1.,-1.E-14,9.60574466455073E-15));
#20040=DIRECTION('',(1.E-14,1.,0.));
#20041=DIRECTION('center_axis',(-1.,1.E-14,-1.E-14));
#20042=DIRECTION('ref_axis',(-1.E-14,-1.,-2.64060752475192E-45));
#20043=DIRECTION('',(1.E-14,1.,0.));
#20044=DIRECTION('center_axis',(-1.E-14,0.,1.));
#20045=DIRECTION('ref_axis',(1.,-1.E-14,1.E-14));
#20046=DIRECTION('center_axis',(-9.60574466455072E-15,-3.94255335449275E-30,
1.));
#20047=DIRECTION('ref_axis',(1.,-1.E-14,9.60574466455072E-15));
#20048=DIRECTION('',(1.E-14,1.,0.));
#20049=DIRECTION('center_axis',(-1.,1.E-14,-1.E-14));
#20050=DIRECTION('ref_axis',(-1.E-14,-1.,-2.64060752475192E-45));
#20051=DIRECTION('',(1.E-14,1.,0.));
#20052=DIRECTION('center_axis',(-1.E-14,0.,1.));
#20053=DIRECTION('ref_axis',(1.,-1.E-14,1.E-14));
#20054=DIRECTION('center_axis',(-9.60574466455072E-15,-3.94255335449275E-30,
1.));
#20055=DIRECTION('ref_axis',(1.,-1.E-14,9.60574466455072E-15));
#20056=DIRECTION('',(1.E-14,1.,0.));
#20057=DIRECTION('center_axis',(-1.,1.E-14,-1.E-14));
#20058=DIRECTION('ref_axis',(-1.E-14,-1.,-2.64060752475192E-45));
#20059=DIRECTION('',(1.E-14,1.,0.));
#20060=DIRECTION('center_axis',(-1.E-14,0.,1.));
#20061=DIRECTION('ref_axis',(1.,-1.E-14,1.E-14));
#20062=DIRECTION('center_axis',(-9.60574466455072E-15,-3.94255335449275E-30,
1.));
#20063=DIRECTION('ref_axis',(1.,-1.E-14,9.60574466455072E-15));
#20064=DIRECTION('',(1.E-14,1.,0.));
#20065=DIRECTION('center_axis',(-1.,1.E-14,-1.E-14));
#20066=DIRECTION('ref_axis',(-1.E-14,-1.,-2.64060752475192E-45));
#20067=DIRECTION('',(1.E-14,1.,0.));
#20068=DIRECTION('center_axis',(-1.E-14,0.,1.));
#20069=DIRECTION('ref_axis',(1.,-1.E-14,1.E-14));
#20070=DIRECTION('center_axis',(-9.60574466455072E-15,-3.94255335449275E-30,
1.));
#20071=DIRECTION('ref_axis',(1.,-1.E-14,9.60574466455072E-15));
#20072=DIRECTION('',(1.E-14,1.,0.));
#20073=DIRECTION('center_axis',(-1.,1.E-14,-1.E-14));
#20074=DIRECTION('ref_axis',(-1.E-14,-1.,-2.64060752475192E-45));
#20075=DIRECTION('',(1.E-14,1.,0.));
#20076=DIRECTION('center_axis',(-1.E-14,0.,1.));
#20077=DIRECTION('ref_axis',(1.,-1.E-14,1.E-14));
#20078=DIRECTION('center_axis',(-9.60574466455072E-15,-3.94255335449275E-30,
1.));
#20079=DIRECTION('ref_axis',(1.,-1.E-14,9.60574466455072E-15));
#20080=DIRECTION('',(1.E-14,1.,0.));
#20081=DIRECTION('center_axis',(-1.,1.E-14,-1.E-14));
#20082=DIRECTION('ref_axis',(-1.E-14,-1.,-2.64060752475192E-45));
#20083=DIRECTION('',(1.E-14,1.,0.));
#20084=DIRECTION('center_axis',(-1.E-14,0.,1.));
#20085=DIRECTION('ref_axis',(1.,-1.E-14,1.E-14));
#20086=DIRECTION('center_axis',(-9.60574466455072E-15,-3.94255335449275E-30,
1.));
#20087=DIRECTION('ref_axis',(1.,-1.E-14,9.60574466455072E-15));
#20088=DIRECTION('',(1.E-14,1.,0.));
#20089=DIRECTION('center_axis',(-1.,1.E-14,-1.E-14));
#20090=DIRECTION('ref_axis',(-1.E-14,-1.,-2.64060752475192E-45));
#20091=DIRECTION('',(1.E-14,1.,0.));
#20092=DIRECTION('center_axis',(-1.E-14,0.,1.));
#20093=DIRECTION('ref_axis',(1.,-1.E-14,1.E-14));
#20094=DIRECTION('center_axis',(-9.60574466455072E-15,-3.94255335449275E-30,
1.));
#20095=DIRECTION('ref_axis',(1.,-1.E-14,9.60574466455072E-15));
#20096=DIRECTION('',(1.E-14,1.,0.));
#20097=DIRECTION('center_axis',(-1.,1.E-14,-1.E-14));
#20098=DIRECTION('ref_axis',(-1.E-14,-1.,-2.64060752475192E-45));
#20099=DIRECTION('',(1.E-14,1.,0.));
#20100=DIRECTION('center_axis',(-1.E-14,0.,1.));
#20101=DIRECTION('ref_axis',(1.,-1.E-14,1.E-14));
#20102=DIRECTION('center_axis',(-9.60574466455072E-15,-3.94255335449275E-30,
1.));
#20103=DIRECTION('ref_axis',(1.,-1.E-14,9.60574466455072E-15));
#20104=DIRECTION('',(1.E-14,1.,0.));
#20105=DIRECTION('center_axis',(-1.,1.E-14,-1.E-14));
#20106=DIRECTION('ref_axis',(-1.E-14,-1.,-2.64060752475192E-45));
#20107=DIRECTION('',(1.E-14,1.,0.));
#20108=DIRECTION('center_axis',(-1.E-14,0.,1.));
#20109=DIRECTION('ref_axis',(1.,-1.E-14,1.E-14));
#20110=DIRECTION('center_axis',(-9.60574466455072E-15,-3.94255335449275E-30,
1.));
#20111=DIRECTION('ref_axis',(1.,-1.E-14,9.60574466455072E-15));
#20112=DIRECTION('',(1.E-14,1.,0.));
#20113=DIRECTION('center_axis',(-1.,1.E-14,-1.E-14));
#20114=DIRECTION('ref_axis',(-1.E-14,-1.,-2.64060752475192E-45));
#20115=DIRECTION('',(1.E-14,1.,0.));
#20116=DIRECTION('center_axis',(-1.E-14,0.,1.));
#20117=DIRECTION('ref_axis',(1.,-1.E-14,1.E-14));
#20118=DIRECTION('center_axis',(-9.60574466455072E-15,-3.94255335449275E-30,
1.));
#20119=DIRECTION('ref_axis',(1.,-1.E-14,9.60574466455072E-15));
#20120=DIRECTION('',(1.E-14,1.,0.));
#20121=DIRECTION('center_axis',(-1.,1.E-14,-1.E-14));
#20122=DIRECTION('ref_axis',(-1.E-14,-1.,-2.64060752475192E-45));
#20123=DIRECTION('',(1.E-14,1.,0.));
#20124=DIRECTION('center_axis',(-1.E-14,0.,1.));
#20125=DIRECTION('ref_axis',(1.,-1.E-14,1.E-14));
#20126=DIRECTION('center_axis',(-9.60574466455072E-15,-3.94255335449275E-30,
1.));
#20127=DIRECTION('ref_axis',(1.,-1.E-14,9.60574466455072E-15));
#20128=DIRECTION('',(1.E-14,1.,0.));
#20129=DIRECTION('center_axis',(-1.,1.E-14,-1.E-14));
#20130=DIRECTION('ref_axis',(-1.E-14,-1.,-2.64060752475192E-45));
#20131=DIRECTION('',(1.E-14,1.,0.));
#20132=DIRECTION('center_axis',(-1.E-14,0.,1.));
#20133=DIRECTION('ref_axis',(1.,-1.E-14,1.E-14));
#20134=DIRECTION('center_axis',(-9.60574466455072E-15,-3.94255335449275E-30,
1.));
#20135=DIRECTION('ref_axis',(1.,-1.E-14,9.60574466455072E-15));
#20136=DIRECTION('',(1.E-14,1.,0.));
#20137=DIRECTION('center_axis',(-1.,1.E-14,-1.E-14));
#20138=DIRECTION('ref_axis',(-1.E-14,-1.,-2.64060752475192E-45));
#20139=DIRECTION('',(1.E-14,1.,0.));
#20140=DIRECTION('center_axis',(-1.E-14,0.,1.));
#20141=DIRECTION('ref_axis',(1.,-1.E-14,1.E-14));
#20142=DIRECTION('center_axis',(-9.60574466455072E-15,-3.94255335449275E-30,
1.));
#20143=DIRECTION('ref_axis',(1.,-1.E-14,9.60574466455072E-15));
#20144=DIRECTION('',(1.E-14,1.,0.));
#20145=DIRECTION('center_axis',(-1.,1.E-14,-1.E-14));
#20146=DIRECTION('ref_axis',(-1.E-14,-1.,-2.64060752475192E-45));
#20147=DIRECTION('',(1.E-14,1.,0.));
#20148=DIRECTION('center_axis',(-1.E-14,0.,1.));
#20149=DIRECTION('ref_axis',(1.,-1.E-14,1.E-14));
#20150=DIRECTION('center_axis',(-9.60574466455072E-15,-3.94255335449275E-30,
1.));
#20151=DIRECTION('ref_axis',(1.,-1.E-14,9.60574466455072E-15));
#20152=DIRECTION('',(1.E-14,1.,0.));
#20153=DIRECTION('center_axis',(-1.,1.E-14,-1.E-14));
#20154=DIRECTION('ref_axis',(-1.E-14,-1.,-2.64060752475192E-45));
#20155=DIRECTION('',(1.E-14,1.,0.));
#20156=DIRECTION('center_axis',(-1.E-14,0.,1.));
#20157=DIRECTION('ref_axis',(1.,-1.E-14,1.E-14));
#20158=DIRECTION('center_axis',(-9.60574466455072E-15,-3.94255335449275E-30,
1.));
#20159=DIRECTION('ref_axis',(1.,-1.E-14,9.60574466455072E-15));
#20160=DIRECTION('',(1.E-14,1.,0.));
#20161=DIRECTION('center_axis',(-1.,1.E-14,-1.E-14));
#20162=DIRECTION('ref_axis',(-1.E-14,-1.,-2.64060752475192E-45));
#20163=DIRECTION('',(1.E-14,1.,0.));
#20164=DIRECTION('center_axis',(-1.E-14,0.,1.));
#20165=DIRECTION('ref_axis',(1.,-1.E-14,1.E-14));
#20166=DIRECTION('center_axis',(1.,-1.E-14,0.));
#20167=DIRECTION('ref_axis',(1.E-14,1.,0.));
#20168=DIRECTION('axis',(0.,0.,1.));
#20169=DIRECTION('refdir',(1.,0.,0.));
#20170=DIRECTION('center_axis',(-2.E-15,0.,-1.));
#20171=DIRECTION('ref_axis',(0.,1.,0.));
#20172=DIRECTION('center_axis',(-0.707106781186422,-2.63949809299824E-13,
-0.707106781186673));
#20173=DIRECTION('ref_axis',(0.707106781186673,5.14283623687556E-12,-0.707106781186422));
#20174=DIRECTION('center_axis',(-0.707106781186407,2.94314808737385E-13,
0.707106781186688));
#20175=DIRECTION('ref_axis',(0.707106781186688,-1.95499137120663E-12,0.707106781186407));
#20176=DIRECTION('',(2.E-15,-2.492418787323E-17,1.));
#20177=DIRECTION('center_axis',(-0.707106781186639,-1.64750638840042E-13,
-0.707106781186456));
#20178=DIRECTION('ref_axis',(0.707106781186456,1.02903869399948E-12,-0.707106781186639));
#20179=DIRECTION('center_axis',(-0.707106781186606,1.10586045248791E-13,
0.707106781186489));
#20180=DIRECTION('ref_axis',(0.707106781186489,-2.4427646214065E-13,0.707106781186606));
#20181=DIRECTION('',(-2.E-15,2.492418787323E-17,-1.));
#20182=DIRECTION('center_axis',(1.,-1.E-15,-2.E-15));
#20183=DIRECTION('ref_axis',(-1.E-15,-1.,2.E-30));
#20184=DIRECTION('',(1.,-1.E-15,-2.E-15));
#20185=DIRECTION('center_axis',(-1.,1.E-15,2.E-15));
#20186=DIRECTION('ref_axis',(2.E-15,-2.E-30,1.));
#20187=DIRECTION('',(-1.,1.E-15,1.7831595655029E-15));
#20188=DIRECTION('center_axis',(-2.E-15,0.,-1.));
#20189=DIRECTION('ref_axis',(-1.,0.,2.E-15));
#20190=DIRECTION('center_axis',(-0.707106781186533,-3.78536648393456E-14,
-0.707106781186562));
#20191=DIRECTION('ref_axis',(0.707106781186562,2.12340059618623E-12,-0.707106781186533));
#20192=DIRECTION('center_axis',(-0.70710678118642,2.63436887012028E-13,
0.707106781186675));
#20193=DIRECTION('ref_axis',(0.707106781186675,4.53699827383031E-13,0.707106781186421));
#20194=DIRECTION('',(1.25746720174781E-15,7.42532798252193E-31,1.));
#20195=DIRECTION('center_axis',(-0.707106781186551,2.46202698142038E-15,
-0.707106781186544));
#20196=DIRECTION('ref_axis',(0.707106781186544,-5.81158480807406E-13,-0.707106781186551));
#20197=DIRECTION('center_axis',(-0.707106781186549,-6.5654052837888E-15,
0.707106781186546));
#20198=DIRECTION('ref_axis',(0.707106781186546,2.87235972405227E-13,0.707106781186549));
#20199=DIRECTION('',(-1.25746720174781E-15,-7.42532798252193E-31,-1.));
#20200=DIRECTION('center_axis',(1.,-1.E-15,-2.E-15));
#20201=DIRECTION('ref_axis',(-2.E-15,2.E-30,-1.));
#20202=DIRECTION('',(1.,-1.E-15,-2.E-15));
#20203=DIRECTION('center_axis',(-1.,1.E-15,2.E-15));
#20204=DIRECTION('ref_axis',(2.E-15,1.68404344971007E-31,1.));
#20205=DIRECTION('',(-1.,1.E-15,2.E-15));
#20206=DIRECTION('center_axis',(-2.E-15,0.,-1.));
#20207=DIRECTION('ref_axis',(8.67361737988403E-16,1.,-1.73472347597681E-30));
#20208=DIRECTION('center_axis',(-0.707106781186533,-3.88795094149376E-14,
-0.707106781186562));
#20209=DIRECTION('ref_axis',(0.707106781186562,1.8346264764677E-13,-0.707106781186533));
#20210=DIRECTION('center_axis',(-0.707106781186432,2.39739877315856E-13,
0.707106781186663));
#20211=DIRECTION('ref_axis',(0.707106781186663,-1.65337637937498E-12,0.707106781186432));
#20212=DIRECTION('',(2.E-15,-4.20505361484229E-17,1.));
#20213=DIRECTION('center_axis',(-0.707106781186573,-9.17105050579052E-14,
-0.707106781186522));
#20214=DIRECTION('ref_axis',(0.707106781186522,1.86047575754184E-12,-0.707106781186573));
#20215=DIRECTION('center_axis',(-0.707106781186607,1.60442091622566E-13,
0.707106781186488));
#20216=DIRECTION('ref_axis',(0.707106781186488,-1.11785938449787E-12,0.707106781186607));
#20217=DIRECTION('',(-2.E-15,4.20505361484229E-17,-1.));
#20218=DIRECTION('center_axis',(1.,-1.E-15,-2.E-15));
#20219=DIRECTION('ref_axis',(-2.E-15,-1.68404344971007E-31,-1.));
#20220=DIRECTION('',(1.,-1.E-15,-2.E-15));
#20221=DIRECTION('center_axis',(-1.,1.E-15,2.E-15));
#20222=DIRECTION('ref_axis',(2.E-15,1.68404344971007E-31,1.));
#20223=DIRECTION('',(-1.,1.E-15,2.E-15));
#20224=DIRECTION('center_axis',(1.,-1.E-15,-2.E-15));
#20225=DIRECTION('ref_axis',(-2.E-15,2.E-30,-1.));
#20226=DIRECTION('center_axis',(2.E-15,0.,1.));
#20227=DIRECTION('ref_axis',(1.,0.,-2.E-15));
#20228=DIRECTION('center_axis',(-1.E-15,-1.,0.));
#20229=DIRECTION('ref_axis',(-1.,1.E-15,0.));
#20230=DIRECTION('center_axis',(-2.E-15,0.,-1.));
#20231=DIRECTION('ref_axis',(1.,0.,-2.E-15));
#20232=DIRECTION('center_axis',(1.E-15,1.,0.));
#20233=DIRECTION('ref_axis',(1.,-1.E-15,0.));
#20234=DIRECTION('center_axis',(-1.E-15,-1.,0.));
#20235=DIRECTION('ref_axis',(-1.,1.E-15,0.));
#20236=DIRECTION('',(1.E-15,1.,0.));
#20237=DIRECTION('center_axis',(-1.E-15,-1.,-2.11758236813575E-19));
#20238=DIRECTION('ref_axis',(-2.11758236813575E-34,-2.11758236813575E-19,
1.));
#20239=DIRECTION('',(-1.E-15,-1.,0.));
#20240=DIRECTION('center_axis',(1.,0.,0.));
#20241=DIRECTION('ref_axis',(0.,0.,1.));
#20242=DIRECTION('center_axis',(-2.E-15,0.,-1.));
#20243=DIRECTION('ref_axis',(-1.,0.,2.E-15));
#20244=DIRECTION('center_axis',(-2.E-15,2.94543590196345E-19,-1.));
#20245=DIRECTION('ref_axis',(5.89087180392689E-34,1.,2.94543590196345E-19));
#20246=DIRECTION('center_axis',(-2.E-15,0.,-1.));
#20247=DIRECTION('ref_axis',(-1.,0.,2.E-15));
#20248=DIRECTION('',(2.E-15,-2.94543590196345E-19,1.));
#20249=DIRECTION('',(-2.E-15,0.,-1.));
#20250=DIRECTION('',(2.E-15,-2.94543590196345E-19,1.));
#20251=DIRECTION('',(-2.E-15,2.94543590196345E-19,-1.));
#20252=DIRECTION('',(-2.E-15,0.,-1.));
#20253=DIRECTION('',(-2.E-15,2.94543590196345E-19,-1.));
#20254=DIRECTION('center_axis',(1.,0.,0.));
#20255=DIRECTION('ref_axis',(0.,0.,1.));
#20256=DIRECTION('center_axis',(1.E-15,1.,0.));
#20257=DIRECTION('ref_axis',(1.,-1.E-15,0.));
#20258=DIRECTION('center_axis',(-1.E-15,-1.,0.));
#20259=DIRECTION('ref_axis',(-1.,1.E-15,0.));
#20260=DIRECTION('center_axis',(1.E-15,1.,0.));
#20261=DIRECTION('ref_axis',(1.,-1.E-15,0.));
#20262=DIRECTION('center_axis',(-1.E-15,-1.,-2.11758236813575E-19));
#20263=DIRECTION('ref_axis',(-2.11758236813575E-34,-2.11758236813575E-19,
1.));
#20264=DIRECTION('',(-1.E-15,-1.,0.));
#20265=DIRECTION('',(1.E-15,1.,0.));
#20266=DIRECTION('center_axis',(-1.,1.E-15,-1.46944695195361E-15));
#20267=DIRECTION('ref_axis',(-1.46944695195361E-15,1.46944695195362E-30,
1.));
#20268=DIRECTION('center_axis',(1.,-1.E-15,-2.E-15));
#20269=DIRECTION('ref_axis',(-2.E-15,2.E-30,-1.));
#20270=DIRECTION('center_axis',(2.E-15,0.,1.));
#20271=DIRECTION('ref_axis',(-1.,0.,2.E-15));
#20272=DIRECTION('center_axis',(-2.E-15,0.,-1.));
#20273=DIRECTION('ref_axis',(-1.,0.,2.E-15));
#20274=DIRECTION('center_axis',(-1.,1.E-15,2.E-15));
#20275=DIRECTION('ref_axis',(2.E-15,-2.E-30,1.));
#20276=DIRECTION('',(1.,-1.E-15,-2.E-15));
#20277=DIRECTION('',(-1.,1.E-15,2.E-15));
#20278=DIRECTION('center_axis',(1.,-1.E-15,-2.E-15));
#20279=DIRECTION('ref_axis',(1.E-15,1.,-2.E-30));
#20280=DIRECTION('center_axis',(-2.E-15,2.E-30,-1.));
#20281=DIRECTION('ref_axis',(1.E-15,1.,0.));
#20282=DIRECTION('',(-1.E-15,-1.,0.));
#20283=DIRECTION('center_axis',(2.E-15,0.,1.));
#20284=DIRECTION('ref_axis',(-1.,0.,2.E-15));
#20285=DIRECTION('',(1.,-1.E-15,-2.E-15));
#20286=DIRECTION('',(1.E-15,1.,0.));
#20287=DIRECTION('',(1.,-1.E-15,-2.E-15));
#20288=DIRECTION('center_axis',(1.E-15,1.,-3.67526160164598E-17));
#20289=DIRECTION('ref_axis',(-2.E-15,-3.67526160164578E-17,-1.));
#20290=DIRECTION('',(-2.E-15,-3.67526160164578E-17,-1.));
#20291=DIRECTION('',(2.E-15,3.67526160164578E-17,1.));
#20292=DIRECTION('',(1.,-1.E-15,-2.E-15));
#20293=DIRECTION('center_axis',(-2.E-15,2.E-30,-1.));
#20294=DIRECTION('ref_axis',(1.E-15,1.,0.));
#20295=DIRECTION('',(-1.E-15,-1.,0.));
#20296=DIRECTION('',(1.E-15,1.,0.));
#20297=DIRECTION('',(1.,-1.E-15,-2.E-15));
#20298=DIRECTION('center_axis',(1.E-15,1.,-2.E-30));
#20299=DIRECTION('ref_axis',(-2.E-15,1.44148758291472E-46,-1.));
#20300=DIRECTION('',(-2.E-15,0.,-1.));
#20301=DIRECTION('',(2.E-15,0.,1.));
#20302=DIRECTION('',(1.,-1.E-15,-2.E-15));
#20303=DIRECTION('center_axis',(2.E-15,0.,1.));
#20304=DIRECTION('ref_axis',(1.,-1.E-15,-2.E-15));
#20305=DIRECTION('',(1.E-15,1.,0.));
#20306=DIRECTION('',(-1.E-15,-1.,0.));
#20307=DIRECTION('',(1.,-1.E-15,-2.E-15));
#20308=DIRECTION('center_axis',(-2.E-15,0.,-1.));
#20309=DIRECTION('ref_axis',(1.,0.,-2.E-15));
#20310=DIRECTION('center_axis',(-1.E-15,-1.,1.23908819712631E-16));
#20311=DIRECTION('ref_axis',(2.E-15,1.23908819712629E-16,1.));
#20312=DIRECTION('',(-2.E-15,-1.23908819712629E-16,-1.));
#20313=DIRECTION('',(-2.E-15,2.11758236813575E-19,-1.));
#20314=DIRECTION('center_axis',(2.E-15,0.,1.));
#20315=DIRECTION('ref_axis',(0.,-1.,0.));
#20316=DIRECTION('center_axis',(-2.E-15,0.,-1.));
#20317=DIRECTION('ref_axis',(0.,1.,0.));
#20318=DIRECTION('',(-2.E-15,1.39036381887169E-17,-1.));
#20319=DIRECTION('center_axis',(2.E-15,-1.88507897725893E-17,1.));
#20320=DIRECTION('ref_axis',(1.,3.77015795451787E-32,-2.E-15));
#20321=DIRECTION('',(2.E-15,-1.39036381887169E-17,1.));
#20322=DIRECTION('center_axis',(-2.E-15,0.,-1.));
#20323=DIRECTION('ref_axis',(0.,1.,0.));
#20324=DIRECTION('',(2.E-15,-2.11758236813575E-19,1.));
#20325=DIRECTION('',(2.E-15,-2.11758236813575E-19,1.));
#20326=DIRECTION('center_axis',(2.E-15,0.,1.));
#20327=DIRECTION('ref_axis',(0.,1.,0.));
#20328=DIRECTION('',(-2.E-15,2.11758236813575E-19,-1.));
#20329=DIRECTION('center_axis',(-2.E-15,1.88507897725893E-17,-1.));
#20330=DIRECTION('ref_axis',(1.,3.77015795451787E-32,-2.E-15));
#20331=DIRECTION('center_axis',(-2.E-15,1.88507897725913E-17,-1.));
#20332=DIRECTION('ref_axis',(1.E-15,1.,1.88507897725894E-17));
#20333=DIRECTION('',(-1.E-15,-1.,-1.88507897725893E-17));
#20334=DIRECTION('',(-1.E-15,-1.,-1.88507897725893E-17));
#20335=DIRECTION('',(1.,-1.E-15,-2.E-15));
#20336=DIRECTION('',(-1.E-15,-1.,-1.88507897725893E-17));
#20337=DIRECTION('',(1.,-1.E-15,-2.E-15));
#20338=DIRECTION('center_axis',(1.,-1.E-15,-2.E-15));
#20339=DIRECTION('ref_axis',(-2.E-15,0.,-1.));
#20340=DIRECTION('',(-1.E-15,-1.,-1.88507897725893E-17));
#20341=DIRECTION('center_axis',(1.7831595655029E-15,-1.88507897725891E-17,
1.));
#20342=DIRECTION('ref_axis',(1.,-1.E-15,-1.7831595655029E-15));
#20343=DIRECTION('',(-1.E-15,-1.,-1.88507897725893E-17));
#20344=DIRECTION('',(-1.,1.E-15,1.7831595655029E-15));
#20345=DIRECTION('',(1.E-15,1.,1.88507897725893E-17));
#20346=DIRECTION('',(-1.,1.E-15,1.7831595655029E-15));
#20347=DIRECTION('center_axis',(-1.,1.E-15,2.E-15));
#20348=DIRECTION('ref_axis',(-1.E-15,-1.,1.44148758291472E-46));
#20349=DIRECTION('center_axis',(2.E-15,0.,1.));
#20350=DIRECTION('ref_axis',(-8.67361737988403E-16,-1.,1.73472347597681E-30));
#20351=DIRECTION('center_axis',(-2.E-15,0.,-1.));
#20352=DIRECTION('ref_axis',(8.67361737988403E-16,1.,-1.73472347597681E-30));
#20353=DIRECTION('',(-2.E-15,1.39036381887169E-17,-1.));
#20354=DIRECTION('center_axis',(2.E-15,0.,1.));
#20355=DIRECTION('ref_axis',(-8.67361737988403E-16,-1.,1.73472347597681E-30));
#20356=DIRECTION('',(2.E-15,-1.39036381887169E-17,1.));
#20357=DIRECTION('center_axis',(2.E-15,-1.39036381887169E-17,1.));
#20358=DIRECTION('ref_axis',(1.,2.78072763774338E-32,-2.E-15));
#20359=DIRECTION('center_axis',(-2.E-15,0.,-1.));
#20360=DIRECTION('ref_axis',(-1.,0.,2.E-15));
#20361=DIRECTION('',(-1.25746720174781E-15,1.39036381887162E-17,-1.));
#20362=DIRECTION('center_axis',(2.E-15,0.,1.));
#20363=DIRECTION('ref_axis',(-8.67361737988403E-16,-1.,1.73472347597681E-30));
#20364=DIRECTION('',(1.25746720174781E-15,-1.39036381887162E-17,1.));
#20365=DIRECTION('center_axis',(-2.E-15,0.,-1.));
#20366=DIRECTION('ref_axis',(1.0842021724855E-15,1.,-2.16840434497101E-30));
#20367=DIRECTION('center_axis',(2.E-15,-2.94543590196344E-19,1.));
#20368=DIRECTION('ref_axis',(1.,5.89087180392688E-34,-2.E-15));
#20369=DIRECTION('',(-2.E-15,2.11758236813575E-19,-1.));
#20370=DIRECTION('center_axis',(-2.E-15,0.,-1.));
#20371=DIRECTION('ref_axis',(1.0842021724855E-15,1.,-2.16840434497101E-30));
#20372=DIRECTION('',(2.E-15,-2.11758236813575E-19,1.));
#20373=DIRECTION('center_axis',(-2.E-15,2.11758236813575E-19,-1.));
#20374=DIRECTION('ref_axis',(-1.,-4.2351647362715E-34,2.E-15));
#20375=DIRECTION('center_axis',(2.E-15,0.,1.));
#20376=DIRECTION('ref_axis',(-1.,0.,2.E-15));
#20377=DIRECTION('',(-1.25746720174781E-15,2.11758236812832E-19,-1.));
#20378=DIRECTION('center_axis',(-2.E-15,0.,-1.));
#20379=DIRECTION('ref_axis',(-1.0842021724855E-15,-1.,2.16840434497101E-30));
#20380=DIRECTION('',(1.25746720174781E-15,-2.11758236812832E-19,1.));
#20381=DIRECTION('center_axis',(1.71087942067053E-15,-2.94543590196055E-19,
1.));
#20382=DIRECTION('ref_axis',(1.,-1.E-15,-1.71087942067053E-15));
#20383=DIRECTION('',(-1.,1.E-15,1.71087942067053E-15));
#20384=DIRECTION('',(1.E-15,1.,2.94543590196345E-19));
#20385=DIRECTION('',(1.,-1.E-15,-1.71087942067053E-15));
#20386=DIRECTION('',(1.E-15,1.,2.94543590196345E-19));
#20387=DIRECTION('center_axis',(1.,-1.E-15,-2.E-15));
#20388=DIRECTION('ref_axis',(-2.E-15,0.,-1.));
#20389=DIRECTION('',(2.E-15,-1.39036381887169E-17,1.));
#20390=DIRECTION('',(-2.E-15,2.94543590196345E-19,-1.));
#20391=DIRECTION('',(1.E-15,1.,2.94543590196345E-19));
#20392=DIRECTION('center_axis',(-2.E-15,2.94543590198344E-19,-1.));
#20393=DIRECTION('ref_axis',(1.E-15,1.,2.94543590196345E-19));
#20394=DIRECTION('',(1.,-1.E-15,-2.E-15));
#20395=DIRECTION('',(-1.,1.E-15,2.E-15));
#20396=DIRECTION('',(1.E-15,1.,2.94543590196345E-19));
#20397=DIRECTION('center_axis',(1.,-1.E-15,-2.E-15));
#20398=DIRECTION('ref_axis',(-2.E-15,0.,-1.));
#20399=DIRECTION('',(2.E-15,-1.39036381887169E-17,1.));
#20400=DIRECTION('',(-2.E-15,2.94543590196345E-19,-1.));
#20401=DIRECTION('',(1.E-15,1.,2.94543590196345E-19));
#20402=DIRECTION('center_axis',(-2.E-15,2.94543590198344E-19,-1.));
#20403=DIRECTION('ref_axis',(1.E-15,1.,2.94543590196345E-19));
#20404=DIRECTION('',(1.,-1.E-15,-2.E-15));
#20405=DIRECTION('',(-1.,1.E-15,2.E-15));
#20406=DIRECTION('',(1.E-15,1.,2.94543590196345E-19));
#20407=DIRECTION('center_axis',(1.,-1.E-15,-2.E-15));
#20408=DIRECTION('ref_axis',(-2.E-15,0.,-1.));
#20409=DIRECTION('',(2.E-15,-1.39036381887169E-17,1.));
#20410=DIRECTION('',(-2.E-15,2.94543590196345E-19,-1.));
#20411=DIRECTION('',(1.E-15,1.,2.94543590196345E-19));
#20412=DIRECTION('center_axis',(-2.E-15,2.94543590198344E-19,-1.));
#20413=DIRECTION('ref_axis',(1.E-15,1.,2.94543590196345E-19));
#20414=DIRECTION('',(1.,-1.E-15,-2.E-15));
#20415=DIRECTION('',(-1.,1.E-15,2.E-15));
#20416=DIRECTION('',(1.E-15,1.,2.94543590196345E-19));
#20417=DIRECTION('center_axis',(-2.E-15,2.94543590198344E-19,-1.));
#20418=DIRECTION('ref_axis',(1.E-15,1.,2.94543590196345E-19));
#20419=DIRECTION('',(1.,-1.E-15,-2.E-15));
#20420=DIRECTION('',(1.E-15,1.,2.94543590196345E-19));
#20421=DIRECTION('',(-1.,1.E-15,2.E-15));
#20422=DIRECTION('',(1.E-15,1.,2.94543590196345E-19));
#20423=DIRECTION('center_axis',(-1.,1.E-15,2.E-15));
#20424=DIRECTION('ref_axis',(-1.E-15,-1.,1.44148758291472E-46));
#20425=DIRECTION('',(-2.E-15,1.39036381887169E-17,-1.));
#20426=DIRECTION('',(1.E-15,1.,2.94543590196345E-19));
#20427=DIRECTION('',(2.E-15,-2.94543590196345E-19,1.));
#20428=DIRECTION('',(1.E-15,1.,2.94543590196345E-19));
#20429=DIRECTION('center_axis',(2.10217463002298E-15,-2.94543590198447E-19,
1.));
#20430=DIRECTION('ref_axis',(1.E-15,1.,2.94543590196345E-19));
#20431=DIRECTION('',(-1.,1.E-15,2.10217463002298E-15));
#20432=DIRECTION('',(1.,-1.E-15,-2.10217463002298E-15));
#20433=DIRECTION('',(1.E-15,1.,2.94543590196345E-19));
#20434=DIRECTION('center_axis',(-2.E-15,2.94543590198344E-19,-1.));
#20435=DIRECTION('ref_axis',(1.E-15,1.,2.94543590196345E-19));
#20436=DIRECTION('',(1.,-1.E-15,-2.E-15));
#20437=DIRECTION('',(1.E-15,1.,2.94543590196345E-19));
#20438=DIRECTION('',(-1.,1.E-15,2.E-15));
#20439=DIRECTION('center_axis',(-1.,1.E-15,1.25746720174781E-15));
#20440=DIRECTION('ref_axis',(-1.E-15,-1.,9.45020606069163E-47));
#20441=DIRECTION('',(-1.E-15,-1.,-1.88507897725893E-17));
#20442=DIRECTION('',(-1.E-15,-1.,-1.88507897725893E-17));
#20443=DIRECTION('center_axis',(1.,-1.E-15,-1.25746720174781E-15));
#20444=DIRECTION('ref_axis',(-1.25746720174781E-15,-7.42532798252193E-31,
-1.));
#20445=DIRECTION('',(-1.E-15,-1.,-1.88507897725893E-17));
#20446=DIRECTION('',(-1.E-15,-1.,-1.88507897725893E-17));
#20447=DIRECTION('center_axis',(2.E-15,-1.88507897725913E-17,1.));
#20448=DIRECTION('ref_axis',(1.E-15,1.,1.88507897725894E-17));
#20449=DIRECTION('',(-1.,1.E-15,2.E-15));
#20450=DIRECTION('',(-1.E-15,-1.,-1.88507897725893E-17));
#20451=DIRECTION('',(-1.,1.E-15,2.E-15));
#20452=DIRECTION('center_axis',(-2.E-15,1.88507897725913E-17,-1.));
#20453=DIRECTION('ref_axis',(1.E-15,1.,1.88507897725894E-17));
#20454=DIRECTION('',(-1.E-15,-1.,-1.88507897725893E-17));
#20455=DIRECTION('',(-1.E-15,-1.,-1.88507897725893E-17));
#20456=DIRECTION('',(1.,-1.E-15,-2.E-15));
#20457=DIRECTION('center_axis',(1.,-1.E-15,-2.E-15));
#20458=DIRECTION('ref_axis',(-2.E-15,0.,-1.));
#20459=DIRECTION('',(-1.E-15,-1.,-1.88507897725893E-17));
#20460=DIRECTION('center_axis',(2.E-15,-1.88507897725913E-17,1.));
#20461=DIRECTION('ref_axis',(1.E-15,1.,1.88507897725894E-17));
#20462=DIRECTION('',(-1.E-15,-1.,-1.88507897725893E-17));
#20463=DIRECTION('',(-1.,1.E-15,2.E-15));
#20464=DIRECTION('center_axis',(-1.,1.E-15,2.E-15));
#20465=DIRECTION('ref_axis',(-1.E-15,-1.,1.44148758291472E-46));
#20466=DIRECTION('',(2.E-15,-1.39036381887169E-17,1.));
#20467=DIRECTION('',(1.E-15,1.,1.0891631049783E-16));
#20468=DIRECTION('',(-2.E-15,4.20505361484229E-17,-1.));
#20469=DIRECTION('center_axis',(-1.,1.E-15,2.E-15));
#20470=DIRECTION('ref_axis',(2.E-15,-2.E-30,1.));
#20471=DIRECTION('center_axis',(-1.,1.E-15,2.E-15));
#20472=DIRECTION('ref_axis',(2.E-15,-2.E-30,1.));
#20473=DIRECTION('',(1.,-1.E-15,-2.E-15));
#20474=DIRECTION('center_axis',(1.,-1.E-15,-2.E-15));
#20475=DIRECTION('ref_axis',(2.E-15,-2.E-30,1.));
#20476=DIRECTION('',(-1.,1.E-15,2.E-15));
#20477=DIRECTION('center_axis',(-1.,1.E-15,2.E-15));
#20478=DIRECTION('ref_axis',(2.E-15,-2.E-30,1.));
#20479=DIRECTION('center_axis',(-1.,1.E-15,2.E-15));
#20480=DIRECTION('ref_axis',(2.E-15,-2.E-30,1.));
#20481=DIRECTION('',(1.,-1.E-15,-2.E-15));
#20482=DIRECTION('center_axis',(1.,-1.E-15,-2.E-15));
#20483=DIRECTION('ref_axis',(2.E-15,-2.E-30,1.));
#20484=DIRECTION('',(-1.,1.E-15,2.E-15));
#20485=DIRECTION('center_axis',(1.,-1.E-15,-2.E-15));
#20486=DIRECTION('ref_axis',(-2.E-15,2.E-30,-1.));
#20487=DIRECTION('center_axis',(-1.,1.E-15,2.E-15));
#20488=DIRECTION('ref_axis',(2.E-15,-2.E-30,1.));
#20489=DIRECTION('',(1.,-1.E-15,-2.E-15));
#20490=DIRECTION('center_axis',(1.,-1.E-15,-2.E-15));
#20491=DIRECTION('ref_axis',(2.E-15,-2.E-30,1.));
#20492=DIRECTION('',(-1.,1.E-15,2.E-15));
#20493=DIRECTION('center_axis',(1.,-1.E-15,-2.E-15));
#20494=DIRECTION('ref_axis',(-2.E-15,2.E-30,-1.));
#20495=DIRECTION('center_axis',(-1.,1.E-15,2.E-15));
#20496=DIRECTION('ref_axis',(2.E-15,-2.E-30,1.));
#20497=DIRECTION('',(1.,-1.E-15,-2.E-15));
#20498=DIRECTION('center_axis',(1.,-1.E-15,-2.E-15));
#20499=DIRECTION('ref_axis',(2.E-15,-2.E-30,1.));
#20500=DIRECTION('',(-1.,1.E-15,2.E-15));
#20501=DIRECTION('center_axis',(2.E-15,-1.39036381887169E-17,1.));
#20502=DIRECTION('ref_axis',(-2.78072763774338E-32,-1.,-1.39036381887169E-17));
#20503=DIRECTION('',(2.E-15,-1.39036381887169E-17,1.));
#20504=DIRECTION('',(-2.E-15,1.39036381887169E-17,-1.));
#20505=DIRECTION('',(2.E-15,-1.39036381887169E-17,1.));
#20506=DIRECTION('',(2.E-15,0.,1.));
#20507=DIRECTION('center_axis',(2.E-15,0.,1.));
#20508=DIRECTION('ref_axis',(1.,-1.E-15,-2.E-15));
#20509=DIRECTION('',(1.E-15,1.,0.));
#20510=DIRECTION('',(1.E-15,1.,0.));
#20511=DIRECTION('center_axis',(1.E-15,1.,-2.E-30));
#20512=DIRECTION('ref_axis',(-2.E-15,1.44148758291472E-46,-1.));
#20513=DIRECTION('center_axis',(-2.E-15,2.E-30,-1.));
#20514=DIRECTION('ref_axis',(1.E-15,1.,0.));
#20515=DIRECTION('',(-1.E-15,-1.,0.));
#20516=DIRECTION('',(-1.E-15,-1.,0.));
#20517=DIRECTION('center_axis',(-1.,1.E-15,2.E-15));
#20518=DIRECTION('ref_axis',(-1.E-15,-1.,1.44148758291472E-46));
#20519=DIRECTION('',(-2.E-15,2.94543590196345E-19,-1.));
#20520=DIRECTION('center_axis',(-1.,1.E-15,2.E-15));
#20521=DIRECTION('ref_axis',(-1.E-15,-1.,1.44148758291472E-46));
#20522=DIRECTION('center_axis',(-2.E-15,2.E-30,-1.));
#20523=DIRECTION('ref_axis',(1.E-15,1.,0.));
#20524=DIRECTION('',(-1.,1.E-15,2.E-15));
#20525=DIRECTION('',(1.E-15,1.,0.));
#20526=DIRECTION('center_axis',(2.E-15,0.,1.));
#20527=DIRECTION('ref_axis',(1.,-1.E-15,-2.E-15));
#20528=DIRECTION('',(-1.E-15,-1.,0.));
#20529=DIRECTION('',(1.,-1.E-15,-2.E-15));
#20530=DIRECTION('center_axis',(-1.E-15,-1.,0.));
#20531=DIRECTION('ref_axis',(-1.,1.E-15,2.E-15));
#20532=DIRECTION('',(-1.,1.E-15,2.E-15));
#20533=DIRECTION('',(2.E-15,0.,1.));
#20534=DIRECTION('',(1.,-1.E-15,-2.E-15));
#20535=DIRECTION('',(2.E-15,0.,1.));
#20536=DIRECTION('center_axis',(1.,-1.E-15,-2.E-15));
#20537=DIRECTION('ref_axis',(-2.E-15,0.,-1.));
#20538=DIRECTION('center_axis',(-1.,1.E-15,2.E-15));
#20539=DIRECTION('ref_axis',(-2.E-15,-1.93999646477936E-30,-1.));
#20540=DIRECTION('',(-2.E-15,2.11758236813575E-19,-1.));
#20541=DIRECTION('',(2.E-15,-1.39036381887169E-17,1.));
#20542=DIRECTION('center_axis',(1.,-1.E-15,-2.E-15));
#20543=DIRECTION('ref_axis',(-2.E-15,-1.22385608907605E-30,-1.));
#20544=DIRECTION('center_axis',(-1.,1.57824115865894E-15,2.E-15));
#20545=DIRECTION('ref_axis',(2.E-15,0.,1.));
#20546=DIRECTION('center_axis',(-1.,1.40298201113451E-15,2.E-15));
#20547=DIRECTION('ref_axis',(1.40298201113451E-15,1.,-2.80596402226901E-30));
#20548=DIRECTION('',(-2.E-15,1.39036381887169E-17,-1.));
#20549=DIRECTION('',(2.E-15,-2.11758236813575E-19,1.));
#20550=DIRECTION('center_axis',(1.,-1.49249955809742E-15,-2.E-15));
#20551=DIRECTION('ref_axis',(1.49249955809742E-15,1.,-2.98499911619484E-30));
#20552=DIRECTION('center_axis',(-8.78027255595381E-16,-1.,1.75605451119076E-30));
#20553=DIRECTION('ref_axis',(2.E-15,1.65592381969512E-47,1.));
#20554=DIRECTION('',(-1.,1.E-15,2.E-15));
#20555=DIRECTION('',(2.E-15,0.,1.));
#20556=DIRECTION('',(1.,-8.78027255595381E-16,-2.E-15));
#20557=DIRECTION('',(2.E-15,0.,1.));
#20558=DIRECTION('center_axis',(1.,-1.E-15,-2.E-15));
#20559=DIRECTION('ref_axis',(-2.E-15,0.,-1.));
#20560=DIRECTION('center_axis',(-1.,1.E-15,2.E-15));
#20561=DIRECTION('ref_axis',(-2.E-15,3.00017676103224E-32,-1.));
#20562=DIRECTION('',(-2.E-15,2.11758236813575E-19,-1.));
#20563=DIRECTION('',(2.E-15,-1.39036381887169E-17,1.));
#20564=DIRECTION('center_axis',(1.,-1.E-15,-2.E-15));
#20565=DIRECTION('ref_axis',(-2.E-15,3.88071955461975E-31,-1.));
#20566=DIRECTION('center_axis',(-1.,1.E-15,2.E-15));
#20567=DIRECTION('ref_axis',(-1.E-15,-1.,1.44148758291472E-46));
#20568=DIRECTION('',(-2.E-15,2.492418787323E-17,-1.));
#20569=DIRECTION('',(2.E-15,-2.11758236813575E-19,1.));
#20570=DIRECTION('center_axis',(1.,-1.E-15,-2.E-15));
#20571=DIRECTION('ref_axis',(2.E-15,-3.93999646477935E-15,1.));
#20572=DIRECTION('center_axis',(-1.,1.E-15,2.E-15));
#20573=DIRECTION('ref_axis',(2.E-15,1.22385608907605E-30,1.));
#20574=DIRECTION('center_axis',(2.E-15,0.,1.));
#20575=DIRECTION('ref_axis',(1.,0.,-2.E-15));
#20576=DIRECTION('',(2.E-15,0.,1.));
#20577=DIRECTION('center_axis',(2.E-15,0.,1.));
#20578=DIRECTION('ref_axis',(1.,0.,-2.E-15));
#20579=DIRECTION('',(2.E-15,0.,1.));
#20580=DIRECTION('center_axis',(2.E-15,-1.35525271560688E-16,1.));
#20581=DIRECTION('ref_axis',(2.71050543121376E-31,1.,1.35525271560688E-16));
#20582=DIRECTION('center_axis',(-1.,1.E-15,2.E-15));
#20583=DIRECTION('ref_axis',(-1.E-15,-1.,1.44148758291472E-46));
#20584=DIRECTION('',(2.E-15,0.,1.));
#20585=DIRECTION('',(-1.E-15,-1.,0.));
#20586=DIRECTION('',(-1.E-15,-1.,-1.0891631049783E-16));
#20587=DIRECTION('center_axis',(2.E-15,0.,1.));
#20588=DIRECTION('ref_axis',(1.,0.,-2.E-15));
#20589=DIRECTION('',(2.E-15,0.,1.));
#20590=DIRECTION('center_axis',(2.E-15,0.,1.));
#20591=DIRECTION('ref_axis',(1.,0.,-2.E-15));
#20592=DIRECTION('center_axis',(2.E-15,-1.35525271560688E-16,1.));
#20593=DIRECTION('ref_axis',(2.71050543121376E-31,1.,1.35525271560688E-16));
#20594=DIRECTION('center_axis',(1.,-1.E-15,-2.E-15));
#20595=DIRECTION('ref_axis',(-2.E-15,0.,-1.));
#20596=DIRECTION('',(1.E-15,1.,0.));
#20597=DIRECTION('',(1.E-15,1.,1.0891631049783E-16));
#20598=DIRECTION('center_axis',(2.E-15,0.,1.));
#20599=DIRECTION('ref_axis',(1.,0.,-2.E-15));
#20600=DIRECTION('',(2.E-15,0.,1.));
#20601=DIRECTION('center_axis',(2.E-15,0.,1.));
#20602=DIRECTION('ref_axis',(1.,0.,-2.E-15));
#20603=DIRECTION('',(2.E-15,0.,1.));
#20604=DIRECTION('center_axis',(2.E-15,-1.35525271560688E-16,1.));
#20605=DIRECTION('ref_axis',(1.0842021724855E-15,1.,1.35525271560686E-16));
#20606=DIRECTION('center_axis',(-1.,1.E-15,2.E-15));
#20607=DIRECTION('ref_axis',(-1.E-15,-1.,1.44148758291472E-46));
#20608=DIRECTION('',(2.E-15,0.,1.));
#20609=DIRECTION('',(-1.E-15,-1.,0.));
#20610=DIRECTION('',(-1.E-15,-1.,-1.0891631049783E-16));
#20611=DIRECTION('center_axis',(2.E-15,0.,1.));
#20612=DIRECTION('ref_axis',(1.,0.,-2.E-15));
#20613=DIRECTION('',(2.E-15,0.,1.));
#20614=DIRECTION('center_axis',(2.E-15,0.,1.));
#20615=DIRECTION('ref_axis',(1.,0.,-2.E-15));
#20616=DIRECTION('center_axis',(2.E-15,-1.35525271560688E-16,1.));
#20617=DIRECTION('ref_axis',(1.0842021724855E-15,1.,1.35525271560686E-16));
#20618=DIRECTION('center_axis',(1.,-1.E-15,-2.E-15));
#20619=DIRECTION('ref_axis',(-2.E-15,0.,-1.));
#20620=DIRECTION('',(1.E-15,1.,0.));
#20621=DIRECTION('',(1.E-15,1.,1.0891631049783E-16));
#20622=DIRECTION('center_axis',(-1.,1.E-15,2.E-15));
#20623=DIRECTION('ref_axis',(-1.E-15,-1.,1.44148758291472E-46));
#20624=DIRECTION('center_axis',(1.,-1.E-15,-2.E-15));
#20625=DIRECTION('ref_axis',(2.E-15,-3.93999646477936E-15,1.));
#20626=DIRECTION('',(-1.E-15,-1.,0.));
#20627=DIRECTION('',(2.E-15,0.,1.));
#20628=DIRECTION('',(-1.E-15,-1.,-1.0891631049783E-16));
#20629=DIRECTION('',(-1.E-15,-1.,-1.0891631049783E-16));
#20630=DIRECTION('center_axis',(-2.E-15,1.08916310497832E-16,-1.));
#20631=DIRECTION('ref_axis',(1.E-15,1.,1.0891631049783E-16));
#20632=DIRECTION('',(-1.,1.E-15,2.E-15));
#20633=DIRECTION('',(1.,-1.E-15,-2.E-15));
#20634=DIRECTION('',(1.E-15,1.,1.0891631049783E-16));
#20635=DIRECTION('center_axis',(1.,-1.E-15,-2.E-15));
#20636=DIRECTION('ref_axis',(-2.E-15,0.,-1.));
#20637=DIRECTION('',(-2.E-15,4.20505361484229E-17,-1.));
#20638=DIRECTION('center_axis',(-1.,1.E-15,2.E-15));
#20639=DIRECTION('ref_axis',(2.E-15,1.49100556725305E-32,1.));
#20640=DIRECTION('center_axis',(-2.E-15,1.08916310497832E-16,-1.));
#20641=DIRECTION('ref_axis',(1.E-15,1.,1.0891631049783E-16));
#20642=DIRECTION('',(1.,-1.E-15,-2.E-15));
#20643=DIRECTION('',(1.E-15,1.,1.0891631049783E-16));
#20644=DIRECTION('',(1.,-1.E-15,-2.E-15));
#20645=DIRECTION('center_axis',(1.,-1.E-15,-2.E-15));
#20646=DIRECTION('ref_axis',(-2.E-15,2.E-30,-1.));
#20647=DIRECTION('',(1.,-1.E-15,-2.E-15));
#20648=DIRECTION('',(1.,-1.E-15,-2.E-15));
#20649=DIRECTION('center_axis',(-1.,1.E-15,2.E-15));
#20650=DIRECTION('ref_axis',(2.E-15,-2.E-30,1.));
#20651=DIRECTION('center_axis',(-1.E-15,-1.,-1.39036381887169E-17));
#20652=DIRECTION('ref_axis',(-1.,1.E-15,2.E-15));
#20653=DIRECTION('',(-2.E-15,1.39036381887169E-17,-1.));
#20654=DIRECTION('',(1.,-1.E-15,-2.E-15));
#20655=DIRECTION('',(-2.E-15,1.39036381887169E-17,-1.));
#20656=DIRECTION('',(-2.E-15,1.39036381887169E-17,-1.));
#20657=DIRECTION('center_axis',(-2.E-15,2.E-30,-1.));
#20658=DIRECTION('ref_axis',(1.E-15,1.,0.));
#20659=DIRECTION('',(1.E-15,1.,0.));
#20660=DIRECTION('',(1.,-1.E-15,-2.E-15));
#20661=DIRECTION('center_axis',(1.E-15,1.,2.11758236811575E-19));
#20662=DIRECTION('ref_axis',(-2.E-15,2.11758236813575E-19,-1.));
#20663=DIRECTION('',(2.E-15,-2.11758236813575E-19,1.));
#20664=DIRECTION('',(1.,-1.E-15,-2.E-15));
#20665=DIRECTION('',(2.E-15,-2.11758236813575E-19,1.));
#20666=DIRECTION('',(2.E-15,-2.11758236813575E-19,1.));
#20667=DIRECTION('',(-2.E-15,2.94543590196345E-19,-1.));
#20668=DIRECTION('',(1.,-1.E-15,-2.E-15));
#20669=DIRECTION('',(1.,-1.E-15,-2.E-15));
#20670=DIRECTION('center_axis',(1.,-1.E-15,-2.E-15));
#20671=DIRECTION('ref_axis',(-2.E-15,2.E-30,-1.));
#20672=DIRECTION('',(1.,-1.E-15,-2.E-15));
#20673=DIRECTION('center_axis',(2.E-15,0.,1.));
#20674=DIRECTION('ref_axis',(1.,-1.E-15,-2.E-15));
#20675=DIRECTION('',(1.,-1.E-15,-2.E-15));
#20676=DIRECTION('',(1.,-1.E-15,-2.E-15));
#20677=DIRECTION('',(-1.E-15,-1.,0.));
#20678=DIRECTION('',(1.,-1.E-15,-2.E-15));
#20679=DIRECTION('center_axis',(-1.E-15,-1.,0.));
#20680=DIRECTION('ref_axis',(-1.,1.E-15,2.E-15));
#20681=DIRECTION('',(-2.E-15,0.,-1.));
#20682=DIRECTION('center_axis',(1.,-1.E-15,-2.E-15));
#20683=DIRECTION('ref_axis',(-2.E-15,2.E-30,-1.));
#20684=DIRECTION('center_axis',(1.,-1.E-15,-2.E-15));
#20685=DIRECTION('ref_axis',(-2.E-15,2.E-30,-1.));
#20686=DIRECTION('center_axis',(1.,-1.E-15,-2.E-15));
#20687=DIRECTION('ref_axis',(-2.E-15,2.E-30,-1.));
#20688=DIRECTION('center_axis',(1.,-1.E-15,-2.E-15));
#20689=DIRECTION('ref_axis',(-2.E-15,0.,-1.));
#20690=DIRECTION('center_axis',(1.,-1.E-15,-2.E-15));
#20691=DIRECTION('ref_axis',(-2.E-15,0.,-1.));
#20692=DIRECTION('center_axis',(1.,-1.E-15,-2.E-15));
#20693=DIRECTION('ref_axis',(-2.E-15,0.,-1.));
#20694=DIRECTION('center_axis',(-1.,1.E-15,2.E-15));
#20695=DIRECTION('ref_axis',(-1.E-15,-1.,1.44148758291472E-46));
#20696=DIRECTION('center_axis',(-1.,1.E-15,2.E-15));
#20697=DIRECTION('ref_axis',(-1.E-15,-1.,1.44148758291472E-46));
#20698=DIRECTION('center_axis',(-1.,1.E-15,2.E-15));
#20699=DIRECTION('ref_axis',(-1.E-15,-1.,1.44148758291472E-46));
#20700=DIRECTION('axis',(0.,0.,1.));
#20701=DIRECTION('refdir',(1.,0.,0.));
#20702=DIRECTION('center_axis',(-0.236333478439914,-0.971672005858196,0.));
#20703=DIRECTION('ref_axis',(0.,0.,1.));
#20704=DIRECTION('center_axis',(0.0754966680796046,-0.997146054050698,-2.74692391220027E-14));
#20705=DIRECTION('ref_axis',(0.997146054050698,0.0754966680796046,1.5942911265521E-28));
#20706=DIRECTION('center_axis',(-0.999339812484074,-0.0363309672909394,
0.));
#20707=DIRECTION('ref_axis',(-0.0363309672909394,0.999339812484074,0.));
#20708=DIRECTION('center_axis',(0.,0.,1.));
#20709=DIRECTION('ref_axis',(-0.236333478439928,-0.971672005858193,0.));
#20710=DIRECTION('center_axis',(-0.23633347843992,-0.971672005858195,0.));
#20711=DIRECTION('ref_axis',(0.,0.,1.));
#20712=DIRECTION('center_axis',(0.,0.,-1.));
#20713=DIRECTION('ref_axis',(-0.236333478439908,-0.971672005858198,0.));
#20714=DIRECTION('center_axis',(-0.415306904260248,0.909681359198796,-5.45231211346703E-15));
#20715=DIRECTION('ref_axis',(-0.909681359198796,-0.415306904260248,1.26922783649562E-28));
#20716=DIRECTION('center_axis',(-0.925012498947632,-0.379936674711269,0.));
#20717=DIRECTION('ref_axis',(0.37993667471127,-0.925012498947632,0.));
#20718=DIRECTION('center_axis',(-0.236333478439914,-0.971672005858196,0.));
#20719=DIRECTION('ref_axis',(0.,0.,1.));
#20720=DIRECTION('center_axis',(0.0028764021739081,-0.0379909888811286,
0.999273941957043));
#20721=DIRECTION('ref_axis',(-0.236178256038945,-0.971033817554429,-0.0362375018464822));
#20722=DIRECTION('center_axis',(-0.0754966680796046,0.997146054050698,-2.85413571912387E-14));
#20723=DIRECTION('ref_axis',(-0.997146054050698,-0.0754966680796046,1.65546549913322E-28));
#20724=DIRECTION('center_axis',(0.993204169284826,0.11638504248931,0.));
#20725=DIRECTION('ref_axis',(0.11638504248931,-0.993204169284826,0.));
#20726=DIRECTION('center_axis',(-0.23633347843992,-0.971672005858195,0.));
#20727=DIRECTION('ref_axis',(0.,0.,1.));
#20728=DIRECTION('center_axis',(0.971672005858197,-0.236333478439911,0.));
#20729=DIRECTION('ref_axis',(0.236333478439911,0.971672005858197,0.));
#20730=DIRECTION('center_axis',(0.274011388509925,0.961726447055951,0.));
#20731=DIRECTION('ref_axis',(-0.961726447055951,0.274011388509925,0.));
#20732=DIRECTION('center_axis',(0.,0.,-1.));
#20733=DIRECTION('ref_axis',(-0.236333478439934,-0.971672005858191,0.));
#20734=DIRECTION('center_axis',(-0.23633347843992,-0.971672005858195,0.));
#20735=DIRECTION('ref_axis',(0.,0.,1.));
#20736=DIRECTION('center_axis',(-0.34095089927767,0.940081105161543,-9.65676829998355E-15));
#20737=DIRECTION('ref_axis',(0.940081105161543,0.34095089927767,-1.40353996739024E-28));
#20738=DIRECTION('center_axis',(0.92501249894764,0.379936674711252,0.));
#20739=DIRECTION('ref_axis',(-0.379936674711251,0.925012498947639,0.));
#20740=DIRECTION('center_axis',(-0.0352437692312558,-0.0144759130295536,
0.999273898724636));
#20741=DIRECTION('ref_axis',(0.971210055190269,-0.236221121175772,0.0308319737898077));
#20742=DIRECTION('center_axis',(-0.23633347843992,-0.971672005858195,0.));
#20743=DIRECTION('ref_axis',(0.,0.,1.));
#20744=DIRECTION('center_axis',(0.198296686754741,0.980142042778542,-9.74044619800714E-16));
#20745=DIRECTION('ref_axis',(0.980142042778542,-0.198296686754741,-1.3764509829553E-29));
#20746=DIRECTION('center_axis',(0.971672005858197,-0.236333478439911,0.));
#20747=DIRECTION('ref_axis',(0.236333478439911,0.971672005858197,0.));
#20748=DIRECTION('center_axis',(0.,0.,1.));
#20749=DIRECTION('ref_axis',(-0.236333478439934,-0.971672005858191,0.));
#20750=DIRECTION('center_axis',(-0.23633347843992,-0.971672005858195,0.));
#20751=DIRECTION('ref_axis',(0.,0.,1.));
#20752=DIRECTION('center_axis',(0.647185832447714,-0.762332275506527,-2.49982082791546E-14));
#20753=DIRECTION('ref_axis',(0.762332275506527,0.647185832447714,1.52661900852052E-28));
#20754=DIRECTION('center_axis',(0.735109640272731,0.677948240486024,0.));
#20755=DIRECTION('ref_axis',(-0.677948240486024,0.735109640272731,0.));
#20756=DIRECTION('center_axis',(0.0246576012256848,-0.0290446488604601,
-0.999273941957043));
#20757=DIRECTION('ref_axis',(0.971210082705378,-0.236221127868081,0.0308310557740814));
#20758=DIRECTION('center_axis',(-0.23633347843992,-0.971672005858195,0.));
#20759=DIRECTION('ref_axis',(0.,0.,1.));
#20760=DIRECTION('center_axis',(-0.0200037109101314,-0.0324264290370445,
-0.999273925532799));
#20761=DIRECTION('ref_axis',(-0.23617825252725,-0.971033803116402,0.0362379116185114));
#20762=DIRECTION('center_axis',(-0.828649631183008,0.559767620303519,3.15597567973487E-15));
#20763=DIRECTION('ref_axis',(-0.559767620303519,-0.828649631183008,-6.36709701349244E-32));
#20764=DIRECTION('center_axis',(-0.525029657457571,-0.851083931695333,0.));
#20765=DIRECTION('ref_axis',(0.851083931695333,-0.525029657457571,0.));
#20766=DIRECTION('center_axis',(-0.23633347843992,-0.971672005858195,0.));
#20767=DIRECTION('ref_axis',(0.,0.,1.));
#20768=DIRECTION('center_axis',(0.,0.,1.));
#20769=DIRECTION('ref_axis',(-0.236333478439934,-0.971672005858191,0.));
#20770=DIRECTION('center_axis',(-0.647185832447714,0.762332275506527,0.));
#20771=DIRECTION('ref_axis',(-0.762332275506527,-0.647185832447714,0.));
#20772=DIRECTION('center_axis',(0.787128084679879,0.616789573767412,0.));
#20773=DIRECTION('ref_axis',(0.616789573767412,-0.787128084679879,0.));
#20774=DIRECTION('center_axis',(-0.23633347843992,-0.971672005858195,0.));
#20775=DIRECTION('ref_axis',(0.,0.,1.));
#20776=DIRECTION('center_axis',(0.870893430543957,-0.491471904217706,3.3389056492716E-15));
#20777=DIRECTION('ref_axis',(0.491471904217706,0.870893430543957,-1.97739864827934E-29));
#20778=DIRECTION('center_axis',(-0.525029657457559,-0.85108393169534,0.));
#20779=DIRECTION('ref_axis',(-0.85108393169534,0.525029657457559,0.));
#20780=DIRECTION('center_axis',(0.,0.,1.));
#20781=DIRECTION('ref_axis',(-0.236333478439934,-0.971672005858191,0.));
#20782=DIRECTION('center_axis',(0.,0.,1.));
#20783=DIRECTION('ref_axis',(-0.330288866442325,-0.943879899512774,0.));
#20784=DIRECTION('center_axis',(0.,0.,1.));
#20785=DIRECTION('ref_axis',(-0.330288866442324,-0.943879899512774,0.));
#20786=DIRECTION('center_axis',(0.943879899512774,-0.330288866442324,0.));
#20787=DIRECTION('ref_axis',(0.330288866442324,0.943879899512774,0.));
#20788=DIRECTION('center_axis',(0.,0.,-1.));
#20789=DIRECTION('ref_axis',(-0.330288866442325,-0.943879899512774,0.));
#20790=DIRECTION('center_axis',(0.,0.,-1.));
#20791=DIRECTION('ref_axis',(0.330288866442325,0.943879899512774,0.));
#20792=DIRECTION('center_axis',(0.,0.,-1.));
#20793=DIRECTION('ref_axis',(0.330288866442324,0.943879899512774,0.));
#20794=DIRECTION('center_axis',(0.,0.,-1.));
#20795=DIRECTION('ref_axis',(0.330288866442324,0.943879899512774,0.));
#20796=DIRECTION('center_axis',(-0.943879899512774,0.330288866442325,0.));
#20797=DIRECTION('ref_axis',(-0.330288866442325,-0.943879899512774,0.));
#20798=DIRECTION('center_axis',(0.,0.,1.));
#20799=DIRECTION('ref_axis',(-0.330288866442324,-0.943879899512774,0.));
#20800=DIRECTION('center_axis',(0.,0.,1.));
#20801=DIRECTION('ref_axis',(-0.330288866442324,-0.943879899512774,0.));
#20802=DIRECTION('center_axis',(0.,0.,1.));
#20803=DIRECTION('ref_axis',(-0.330288866442324,-0.943879899512774,0.));
#20804=DIRECTION('center_axis',(0.943879899512774,-0.330288866442324,0.));
#20805=DIRECTION('ref_axis',(0.330288866442324,0.943879899512774,0.));
#20806=DIRECTION('center_axis',(0.,0.,-1.));
#20807=DIRECTION('ref_axis',(0.330288866442325,0.943879899512774,0.));
#20808=DIRECTION('center_axis',(0.,0.,-1.));
#20809=DIRECTION('ref_axis',(0.330288866442325,0.943879899512774,0.));
#20810=DIRECTION('center_axis',(0.,0.,1.));
#20811=DIRECTION('ref_axis',(-0.330288866442324,-0.943879899512774,0.));
#20812=DIRECTION('center_axis',(0.,0.,1.));
#20813=DIRECTION('ref_axis',(-0.330288866442324,-0.943879899512774,0.));
#20814=DIRECTION('center_axis',(-0.943879899512774,0.330288866442325,0.));
#20815=DIRECTION('ref_axis',(0.330288866442325,0.943879899512774,0.));
#20816=DIRECTION('center_axis',(0.,0.,-1.));
#20817=DIRECTION('ref_axis',(-0.330288866442325,-0.943879899512774,0.));
#20818=DIRECTION('center_axis',(0.,0.,-1.));
#20819=DIRECTION('ref_axis',(0.330288866442324,0.943879899512774,0.));
#20820=DIRECTION('center_axis',(0.,0.,-1.));
#20821=DIRECTION('ref_axis',(0.330288866442324,0.943879899512774,0.));
#20822=DIRECTION('center_axis',(-0.943879899512774,0.330288866442325,0.));
#20823=DIRECTION('ref_axis',(-0.330288866442325,-0.943879899512774,0.));
#20824=DIRECTION('center_axis',(0.,0.,1.));
#20825=DIRECTION('ref_axis',(0.330288866442325,0.943879899512774,0.));
#20826=DIRECTION('center_axis',(0.,0.,1.));
#20827=DIRECTION('ref_axis',(0.330288866442325,0.943879899512774,0.));
#20828=DIRECTION('center_axis',(0.,0.,1.));
#20829=DIRECTION('ref_axis',(-0.330288866442325,-0.943879899512774,0.));
#20830=DIRECTION('center_axis',(0.,0.,1.));
#20831=DIRECTION('ref_axis',(-0.330288866442324,-0.943879899512774,0.));
#20832=DIRECTION('center_axis',(-0.943879899512774,0.330288866442324,0.));
#20833=DIRECTION('ref_axis',(0.330288866442324,0.943879899512774,0.));
#20834=DIRECTION('center_axis',(0.,0.,-1.));
#20835=DIRECTION('ref_axis',(-0.330288866442325,-0.943879899512774,0.));
#20836=DIRECTION('center_axis',(0.,0.,1.));
#20837=DIRECTION('ref_axis',(-0.330288866442324,-0.943879899512774,0.));
#20838=DIRECTION('center_axis',(0.,0.,1.));
#20839=DIRECTION('ref_axis',(-0.330288866442324,-0.943879899512774,0.));
#20840=DIRECTION('center_axis',(0.943879899512774,-0.330288866442325,0.));
#20841=DIRECTION('ref_axis',(0.330288866442325,0.943879899512774,0.));
#20842=DIRECTION('center_axis',(0.,0.,-1.));
#20843=DIRECTION('ref_axis',(-0.330288866442325,-0.943879899512774,0.));
#20844=DIRECTION('center_axis',(0.,0.,1.));
#20845=DIRECTION('ref_axis',(-0.330288866442324,-0.943879899512774,0.));
#20846=DIRECTION('center_axis',(0.,0.,1.));
#20847=DIRECTION('ref_axis',(0.330288866442325,0.943879899512774,0.));
#20848=DIRECTION('center_axis',(-0.943879899512774,0.330288866442324,0.));
#20849=DIRECTION('ref_axis',(0.330288866442324,0.943879899512774,0.));
#20850=DIRECTION('center_axis',(0.,0.,-1.));
#20851=DIRECTION('ref_axis',(-0.330288866442325,-0.943879899512774,0.));
#20852=DIRECTION('center_axis',(0.,0.,1.));
#20853=DIRECTION('ref_axis',(-0.330288866442324,-0.943879899512774,0.));
#20854=DIRECTION('center_axis',(0.,0.,1.));
#20855=DIRECTION('ref_axis',(-0.330288866442325,-0.943879899512774,0.));
#20856=DIRECTION('center_axis',(-0.943879899512774,0.330288866442325,0.));
#20857=DIRECTION('ref_axis',(0.330288866442324,0.943879899512774,0.));
#20858=DIRECTION('center_axis',(0.,0.,-1.));
#20859=DIRECTION('ref_axis',(-0.330288866442324,-0.943879899512774,0.));
#20860=DIRECTION('center_axis',(0.,0.,1.));
#20861=DIRECTION('ref_axis',(-0.330288866442324,-0.943879899512774,0.));
#20862=DIRECTION('',(0.,0.,-1.));
#20863=DIRECTION('center_axis',(0.,0.,1.));
#20864=DIRECTION('ref_axis',(-0.330288866442325,-0.943879899512774,0.));
#20865=DIRECTION('',(0.,0.,-1.));
#20866=DIRECTION('center_axis',(0.,0.,-1.));
#20867=DIRECTION('ref_axis',(-1.,0.,0.));
#20868=DIRECTION('center_axis',(0.,0.,1.));
#20869=DIRECTION('ref_axis',(-0.330288866442325,-0.943879899512774,0.));
#20870=DIRECTION('center_axis',(0.,0.,-1.));
#20871=DIRECTION('ref_axis',(-1.,0.,0.));
#20872=DIRECTION('center_axis',(0.,0.,1.));
#20873=DIRECTION('ref_axis',(-0.330288866442325,-0.943879899512774,0.));
#20874=DIRECTION('center_axis',(0.,0.,-1.));
#20875=DIRECTION('ref_axis',(-1.,0.,0.));
#20876=DIRECTION('center_axis',(0.,0.,1.));
#20877=DIRECTION('ref_axis',(-0.330288866442325,-0.943879899512774,0.));
#20878=DIRECTION('center_axis',(0.,0.,-1.));
#20879=DIRECTION('ref_axis',(-1.,0.,0.));
#20880=DIRECTION('center_axis',(0.,0.,1.));
#20881=DIRECTION('ref_axis',(-0.330288866442325,-0.943879899512774,0.));
#20882=DIRECTION('center_axis',(0.,0.,-1.));
#20883=DIRECTION('ref_axis',(-1.,0.,0.));
#20884=DIRECTION('center_axis',(0.,0.,1.));
#20885=DIRECTION('ref_axis',(-0.330288866442325,-0.943879899512774,0.));
#20886=DIRECTION('center_axis',(0.,0.,-1.));
#20887=DIRECTION('ref_axis',(-1.,0.,0.));
#20888=DIRECTION('center_axis',(0.,0.,1.));
#20889=DIRECTION('ref_axis',(-0.330288866442324,-0.943879899512774,0.));
#20890=DIRECTION('center_axis',(0.,0.,-1.));
#20891=DIRECTION('ref_axis',(-1.,0.,0.));
#20892=DIRECTION('center_axis',(0.,0.,-1.));
#20893=DIRECTION('ref_axis',(-1.,0.,0.));
#20894=DIRECTION('center_axis',(0.,0.,-1.));
#20895=DIRECTION('ref_axis',(-1.,0.,0.));
#20896=DIRECTION('center_axis',(0.,0.,-1.));
#20897=DIRECTION('ref_axis',(-1.,0.,0.));
#20898=DIRECTION('',(-0.014665028342131,-0.0419088467226302,-0.999013806466209));
#20899=DIRECTION('center_axis',(0.,0.,-1.));
#20900=DIRECTION('ref_axis',(-1.,0.,0.));
#20901=DIRECTION('center_axis',(0.,0.,-1.));
#20902=DIRECTION('ref_axis',(-1.,0.,0.));
#20903=DIRECTION('center_axis',(0.,0.,-1.));
#20904=DIRECTION('ref_axis',(-1.,0.,0.));
#20905=DIRECTION('center_axis',(0.,0.,1.));
#20906=DIRECTION('ref_axis',(-0.330288866442325,-0.943879899512774,0.));
#20907=DIRECTION('center_axis',(0.,0.,1.));
#20908=DIRECTION('ref_axis',(-0.330288866442324,-0.943879899512774,0.));
#20909=DIRECTION('',(0.,0.,1.));
#20910=DIRECTION('center_axis',(0.,0.,1.));
#20911=DIRECTION('ref_axis',(-0.330288866442325,-0.943879899512774,0.));
#20912=DIRECTION('center_axis',(0.,0.,1.));
#20913=DIRECTION('ref_axis',(-0.330288866442325,-0.943879899512774,0.));
#20914=DIRECTION('',(0.,0.,1.));
#20915=DIRECTION('center_axis',(0.,0.,-1.));
#20916=DIRECTION('ref_axis',(0.943879899512774,-0.330288866442325,0.));
#20917=DIRECTION('center_axis',(0.,0.,1.));
#20918=DIRECTION('ref_axis',(-0.330288866442324,-0.943879899512774,0.));
#20919=DIRECTION('center_axis',(0.,0.,1.));
#20920=DIRECTION('ref_axis',(-0.330288866442324,-0.943879899512774,0.));
#20921=DIRECTION('',(0.,0.,-1.));
#20922=DIRECTION('center_axis',(0.,0.,-1.));
#20923=DIRECTION('ref_axis',(0.330288866442324,0.943879899512774,0.));
#20924=DIRECTION('',(0.330247702396689,0.94376226334878,0.0157875058352114));
#20925=DIRECTION('center_axis',(0.,0.,1.));
#20926=DIRECTION('ref_axis',(-0.330288866442325,-0.943879899512774,0.));
#20927=DIRECTION('center_axis',(0.,0.,1.));
#20928=DIRECTION('ref_axis',(-0.236333478439911,-0.971672005858197,0.));
#20929=DIRECTION('center_axis',(0.,0.,1.));
#20930=DIRECTION('ref_axis',(-0.236333478439911,-0.971672005858197,0.));
#20931=DIRECTION('center_axis',(0.,0.,1.));
#20932=DIRECTION('ref_axis',(-0.236333478439911,-0.971672005858197,0.));
#20933=DIRECTION('center_axis',(-0.971672005858197,0.236333478439911,0.));
#20934=DIRECTION('ref_axis',(0.236333478439911,0.971672005858197,0.));
#20935=DIRECTION('center_axis',(0.,0.,-1.));
#20936=DIRECTION('ref_axis',(-0.236333478439911,-0.971672005858197,0.));
#20937=DIRECTION('center_axis',(0.,0.,-1.));
#20938=DIRECTION('ref_axis',(0.236333478439911,0.971672005858197,0.));
#20939=DIRECTION('center_axis',(0.,0.,-1.));
#20940=DIRECTION('ref_axis',(0.236333478439911,0.971672005858197,0.));
#20941=DIRECTION('center_axis',(0.971672005858197,-0.236333478439911,0.));
#20942=DIRECTION('ref_axis',(-0.236333478439911,-0.971672005858197,0.));
#20943=DIRECTION('center_axis',(0.,0.,1.));
#20944=DIRECTION('ref_axis',(0.236333478439911,0.971672005858197,0.));
#20945=DIRECTION('center_axis',(0.,0.,1.));
#20946=DIRECTION('ref_axis',(-0.236333478439911,-0.971672005858197,0.));
#20947=DIRECTION('center_axis',(0.,0.,1.));
#20948=DIRECTION('ref_axis',(-0.236333478439911,-0.971672005858197,0.));
#20949=DIRECTION('center_axis',(0.,0.,1.));
#20950=DIRECTION('ref_axis',(-0.236333478439911,-0.971672005858197,0.));
#20951=DIRECTION('center_axis',(-0.971672005858197,0.236333478439911,0.));
#20952=DIRECTION('ref_axis',(0.236333478439911,0.971672005858197,0.));
#20953=DIRECTION('center_axis',(0.,0.,-1.));
#20954=DIRECTION('ref_axis',(0.236333478439911,0.971672005858197,0.));
#20955=DIRECTION('center_axis',(-0.525029657457558,-0.851083931695341,0.));
#20956=DIRECTION('ref_axis',(0.851083931695341,-0.525029657457558,0.));
#20957=DIRECTION('',(0.525029657457553,0.851083931695343,0.));
#20958=DIRECTION('center_axis',(0.525029657457559,0.85108393169534,2.96134752604748E-14));
#20959=DIRECTION('ref_axis',(0.85108393169534,-0.525029657457559,-7.40770614500254E-28));
#20960=DIRECTION('',(-0.525029657457553,-0.851083931695343,0.));
#20961=DIRECTION('center_axis',(0.,0.,1.));
#20962=DIRECTION('ref_axis',(1.,0.,0.));
#20963=DIRECTION('center_axis',(0.0200037109101317,0.0324264290370445,0.999273925532799));
#20964=DIRECTION('ref_axis',(-0.23617825252725,-0.971033803116402,0.0362379116185115));
#20965=DIRECTION('center_axis',(0.872062858341818,-0.489393881347834,0.));
#20966=DIRECTION('ref_axis',(0.489393881347834,0.872062858341818,0.));
#20967=DIRECTION('center_axis',(0.,0.,-1.));
#20968=DIRECTION('ref_axis',(0.236333478439912,0.971672005858197,0.));
#20969=DIRECTION('center_axis',(0.,0.,-1.));
#20970=DIRECTION('ref_axis',(0.236333478439911,0.971672005858197,0.));
#20971=DIRECTION('center_axis',(0.788606312050867,0.61489843437232,-2.04787185540381E-15));
#20972=DIRECTION('ref_axis',(0.61489843437232,-0.788606312050867,5.79335698387264E-29));
#20973=DIRECTION('center_axis',(-0.0200042106442368,-0.0324272391163663,
-0.999273889241479));
#20974=DIRECTION('ref_axis',(0.851083931702766,-0.525029657445522,-5.68435167261249E-13));
#20975=DIRECTION('',(0.0199847256250061,0.0324383169330875,0.999273919571727));
#20976=DIRECTION('',(-0.526267548714368,-0.850319038461532,-1.61440824337016E-7));
#20977=DIRECTION('',(-0.0200040683734365,-0.0324270084924563,-0.999273899573456));
#20978=DIRECTION('center_axis',(0.,0.,-1.));
#20979=DIRECTION('ref_axis',(0.236333478439934,0.971672005858191,0.));
#20980=DIRECTION('',(0.,0.,-1.));
#20981=DIRECTION('',(0.,0.,1.));
#20982=DIRECTION('center_axis',(0.,0.,-1.));
#20983=DIRECTION('ref_axis',(0.236333478439934,0.971672005858191,0.));
#20984=DIRECTION('center_axis',(0.,0.,-1.));
#20985=DIRECTION('ref_axis',(0.236333478439911,0.971672005858197,0.));
#20986=DIRECTION('center_axis',(0.,0.,1.));
#20987=DIRECTION('ref_axis',(0.236333478439915,0.971672005858196,0.));
#20988=DIRECTION('center_axis',(0.,0.,-1.));
#20989=DIRECTION('ref_axis',(0.236333478439911,0.971672005858197,0.));
#20990=DIRECTION('center_axis',(0.,0.,1.));
#20991=DIRECTION('ref_axis',(1.,0.,0.));
#20992=DIRECTION('center_axis',(-0.0246581606679246,0.0290453078379217,
0.999273908998466));
#20993=DIRECTION('ref_axis',(0.971210061729006,-0.236221122766167,0.0308317556333084));
#20994=DIRECTION('center_axis',(0.647185832447695,-0.762332275506543,0.));
#20995=DIRECTION('ref_axis',(0.762332275506543,0.647185832447695,0.));
#20996=DIRECTION('center_axis',(0.,0.,-1.));
#20997=DIRECTION('ref_axis',(0.236333478439911,0.971672005858197,0.));
#20998=DIRECTION('center_axis',(0.,0.,-1.));
#20999=DIRECTION('ref_axis',(0.236333478439911,0.971672005858197,0.));
#21000=DIRECTION('center_axis',(0.,0.,1.));
#21001=DIRECTION('ref_axis',(0.236333478439904,0.971672005858199,0.));
#21002=DIRECTION('center_axis',(0.,0.,-1.));
#21003=DIRECTION('ref_axis',(0.236333478439911,0.971672005858197,0.));
#21004=DIRECTION('center_axis',(0.,0.,-1.));
#21005=DIRECTION('ref_axis',(0.236333478439911,0.971672005858197,0.));
#21006=DIRECTION('center_axis',(0.,0.,1.));
#21007=DIRECTION('ref_axis',(0.23633347843988,0.971672005858205,0.));
#21008=DIRECTION('center_axis',(-0.647185832447714,0.762332275506527,0.));
#21009=DIRECTION('ref_axis',(-0.762332275506527,-0.647185832447714,0.));
#21010=DIRECTION('',(-0.647185832447714,0.762332275506527,0.));
#21011=DIRECTION('',(0.647185832447714,-0.762332275506527,0.));
#21012=DIRECTION('center_axis',(-0.0246584553606204,0.0290456549619493,
0.999273891636852));
#21013=DIRECTION('ref_axis',(-0.762332275500488,-0.647185832454827,4.26326374061232E-13));
#21014=DIRECTION('',(-0.0246586071825858,0.0290458337958772,0.999273882692286));
#21015=DIRECTION('',(-0.648187897113365,0.761480433127297,1.32007699339018E-7));
#21016=DIRECTION('',(0.0246410696828602,-0.0290600164161832,-0.99927390295693));
#21017=DIRECTION('center_axis',(0.0200039468311077,0.0324268114698234,0.999273908400034));
#21018=DIRECTION('ref_axis',(-0.851083931689181,0.525029657467544,-4.26326364282818E-13));
#21019=DIRECTION('',(-0.0200228534542546,-0.0324147960551628,-0.999273919571732));
#21020=DIRECTION('',(0.0200040683734419,0.0324270084924578,0.999273899573456));
#21021=DIRECTION('',(0.523790654476959,0.851847022817227,1.61489583376044E-7));
#21022=DIRECTION('center_axis',(0.,0.,-1.));
#21023=DIRECTION('ref_axis',(0.236333478439934,0.971672005858191,0.));
#21024=DIRECTION('center_axis',(0.,0.,-1.));
#21025=DIRECTION('ref_axis',(-0.236333478439934,-0.971672005858191,0.));
#21026=DIRECTION('',(0.,0.,1.));
#21027=DIRECTION('center_axis',(0.,0.,-1.));
#21028=DIRECTION('ref_axis',(0.236333478439934,0.971672005858191,0.));
#21029=DIRECTION('',(0.,0.,-1.));
#21030=DIRECTION('center_axis',(0.,0.,-1.));
#21031=DIRECTION('ref_axis',(0.236333478439934,0.971672005858191,0.));
#21032=DIRECTION('center_axis',(0.,0.,-1.));
#21033=DIRECTION('ref_axis',(0.236333478439934,0.971672005858191,0.));
#21034=DIRECTION('',(0.,0.,-1.));
#21035=DIRECTION('',(0.,0.,1.));
#21036=DIRECTION('center_axis',(0.,0.,-1.));
#21037=DIRECTION('ref_axis',(0.236333478439911,0.971672005858197,0.));
#21038=DIRECTION('center_axis',(0.,0.,1.));
#21039=DIRECTION('ref_axis',(0.236333478439911,0.971672005858197,0.));
#21040=DIRECTION('center_axis',(0.,0.,-1.));
#21041=DIRECTION('ref_axis',(0.236333478439911,0.971672005858197,0.));
#21042=DIRECTION('center_axis',(1.,0.,0.));
#21043=DIRECTION('ref_axis',(0.,-1.,0.));
#21044=DIRECTION('center_axis',(-0.82998202866415,0.557790132661507,0.));
#21045=DIRECTION('ref_axis',(-0.557790132661507,-0.82998202866415,0.));
#21046=DIRECTION('center_axis',(0.525029657457559,0.85108393169534,0.));
#21047=DIRECTION('ref_axis',(-0.85108393169534,0.525029657457559,0.));
#21048=DIRECTION('center_axis',(0.,0.,-1.));
#21049=DIRECTION('ref_axis',(0.236333478439911,0.971672005858197,0.));
#21050=DIRECTION('center_axis',(0.,0.,1.));
#21051=DIRECTION('ref_axis',(0.236333478439911,0.971672005858197,0.));
#21052=DIRECTION('center_axis',(0.,0.,-1.));
#21053=DIRECTION('ref_axis',(0.236333478439911,0.971672005858197,0.));
#21054=DIRECTION('center_axis',(0.0246582090638531,-0.0290453648443879,
-0.999273906147268));
#21055=DIRECTION('ref_axis',(0.762332275496643,0.647185832459356,-5.68435154081849E-13));
#21056=DIRECTION('',(-0.0246746594650707,0.0290303609984873,0.999273936075879));
#21057=DIRECTION('',(0.645969033808723,-0.763363614118585,-1.94028037441531E-7));
#21058=DIRECTION('',(0.0246580360155412,-0.0290451610075496,-0.999273916342212));
#21059=DIRECTION('center_axis',(0.,0.,-1.));
#21060=DIRECTION('ref_axis',(0.236333478439912,0.971672005858197,0.));
#21061=DIRECTION('center_axis',(0.19595899650011,0.980612090324543,0.));
#21062=DIRECTION('ref_axis',(0.980612090324543,-0.19595899650011,0.));
#21063=DIRECTION('center_axis',(0.,0.,-1.));
#21064=DIRECTION('ref_axis',(0.236333478439911,0.971672005858197,0.));
#21065=DIRECTION('center_axis',(0.525029657457558,0.851083931695341,0.));
#21066=DIRECTION('ref_axis',(-0.851083931695341,0.525029657457558,0.));
#21067=DIRECTION('',(-0.525029657457553,-0.851083931695343,0.));
#21068=DIRECTION('',(0.525029657457554,0.851083931695343,0.));
#21069=DIRECTION('center_axis',(0.,0.,-1.));
#21070=DIRECTION('ref_axis',(0.236333478439911,0.971672005858197,0.));
#21071=DIRECTION('center_axis',(0.,0.,-1.));
#21072=DIRECTION('ref_axis',(0.236333478439911,0.971672005858197,0.));
#21073=DIRECTION('center_axis',(0.,0.,1.));
#21074=DIRECTION('ref_axis',(0.236333478439915,0.971672005858196,0.));
#21075=DIRECTION('center_axis',(0.,0.,-1.));
#21076=DIRECTION('ref_axis',(0.236333478439934,0.971672005858191,0.));
#21077=DIRECTION('center_axis',(0.,0.,-1.));
#21078=DIRECTION('ref_axis',(-0.236333478439934,-0.971672005858191,0.));
#21079=DIRECTION('',(0.,0.,1.));
#21080=DIRECTION('center_axis',(0.,0.,-1.));
#21081=DIRECTION('ref_axis',(0.236333478439934,0.971672005858191,0.));
#21082=DIRECTION('',(0.,0.,-1.));
#21083=DIRECTION('center_axis',(0.,0.,1.));
#21084=DIRECTION('ref_axis',(-0.843255399479467,-0.537513098676418,0.));
#21085=DIRECTION('center_axis',(0.0370208532576562,-0.00900434197182349,
0.999273925532799));
#21086=DIRECTION('ref_axis',(0.970966499624253,-0.236161882735454,-0.0381001542027123));
#21087=DIRECTION('center_axis',(-0.971672005858197,0.236333478439911,-2.77555756156289E-14));
#21088=DIRECTION('ref_axis',(-2.6969315832187E-14,6.55957173134355E-15,
1.));
#21089=DIRECTION('center_axis',(1.,0.,0.));
#21090=DIRECTION('ref_axis',(0.,-1.,0.));
#21091=DIRECTION('center_axis',(-0.647185832447725,0.762332275506517,0.));
#21092=DIRECTION('ref_axis',(-0.762332275506517,-0.647185832447725,0.));
#21093=DIRECTION('center_axis',(0.736713387417931,0.676205135147019,-7.7165199669874E-15));
#21094=DIRECTION('ref_axis',(-0.676205135147019,0.736713387417931,-1.538061318188E-28));
#21095=DIRECTION('center_axis',(0.647185832447714,-0.762332275506527,0.));
#21096=DIRECTION('ref_axis',(0.762332275506527,0.647185832447714,0.));
#21097=DIRECTION('',(-0.647185832447714,0.762332275506527,0.));
#21098=DIRECTION('',(0.647185832447714,-0.762332275506527,0.));
#21099=DIRECTION('center_axis',(0.,0.,-1.));
#21100=DIRECTION('ref_axis',(0.236333478439912,0.971672005858197,0.));
#21101=DIRECTION('center_axis',(0.,0.,-1.));
#21102=DIRECTION('ref_axis',(0.236333478439911,0.971672005858197,0.));
#21103=DIRECTION('center_axis',(-0.037021778116286,0.00900456691918861,
-0.999273889241436));
#21104=DIRECTION('ref_axis',(-0.236333478439919,-0.971672005858195,0.));
#21105=DIRECTION('',(0.0370262925428981,-0.00898261233079703,0.999273919571727));
#21106=DIRECTION('',(-0.971327078599407,0.237747147994493,-1.61440824441445E-7));
#21107=DIRECTION('',(-0.0370215148147375,0.00900450287806102,-0.999273899573456));
#21108=DIRECTION('center_axis',(-0.971672005858197,0.236333478439911,0.));
#21109=DIRECTION('ref_axis',(-0.236333478439911,-0.971672005858197,0.));
#21110=DIRECTION('',(-0.971672005858197,0.236333478439911,0.));
#21111=DIRECTION('',(0.971672005858197,-0.236333478439911,0.));
#21112=DIRECTION('center_axis',(0.,0.,-1.));
#21113=DIRECTION('ref_axis',(0.236333478439934,0.971672005858191,0.));
#21114=DIRECTION('',(0.,0.,-1.));
#21115=DIRECTION('',(0.,0.,1.));
#21116=DIRECTION('center_axis',(0.,0.,-1.));
#21117=DIRECTION('ref_axis',(0.236333478439934,0.971672005858191,0.));
#21118=DIRECTION('center_axis',(0.,0.,-1.));
#21119=DIRECTION('ref_axis',(0.236333478439911,0.971672005858197,0.));
#21120=DIRECTION('center_axis',(-0.34321561568671,0.939256642855824,0.));
#21121=DIRECTION('ref_axis',(0.939256642855824,0.34321561568671,0.));
#21122=DIRECTION('center_axis',(0.,0.,1.));
#21123=DIRECTION('ref_axis',(0.236333478439911,0.971672005858197,0.));
#21124=DIRECTION('center_axis',(0.,0.,-1.));
#21125=DIRECTION('ref_axis',(0.236333478439911,0.971672005858197,0.));
#21126=DIRECTION('center_axis',(0.,0.,-1.));
#21127=DIRECTION('ref_axis',(0.236333478439911,0.971672005858197,0.));
#21128=DIRECTION('center_axis',(0.,0.,-1.));
#21129=DIRECTION('ref_axis',(0.236333478439911,0.971672005858197,0.));
#21130=DIRECTION('center_axis',(0.,0.,1.));
#21131=DIRECTION('ref_axis',(0.236333478439911,0.971672005858197,0.));
#21132=DIRECTION('center_axis',(0.,0.,-1.));
#21133=DIRECTION('ref_axis',(0.236333478439911,0.971672005858197,0.));
#21134=DIRECTION('center_axis',(0.,0.,-1.));
#21135=DIRECTION('ref_axis',(0.236333478439911,0.971672005858197,0.));
#21136=DIRECTION('center_axis',(0.,0.,1.));
#21137=DIRECTION('ref_axis',(0.236333478439891,0.971672005858202,0.));
#21138=DIRECTION('center_axis',(1.,0.,0.));
#21139=DIRECTION('ref_axis',(0.,-1.,0.));
#21140=DIRECTION('center_axis',(0.,0.,1.));
#21141=DIRECTION('ref_axis',(-0.236333478439908,-0.971672005858198,0.));
#21142=DIRECTION('center_axis',(-0.925012498947636,-0.37993667471126,4.07857950393881E-15));
#21143=DIRECTION('ref_axis',(0.37993667471126,-0.925012498947636,-5.72282343898698E-29));
#21144=DIRECTION('center_axis',(-0.925012498947636,-0.37993667471126,0.));
#21145=DIRECTION('ref_axis',(0.37993667471126,-0.925012498947636,0.));
#21146=DIRECTION('',(-0.925012498947635,-0.379936674711261,0.));
#21147=DIRECTION('',(0.925012498947635,0.379936674711261,0.));
#21148=DIRECTION('center_axis',(-0.0352441938793423,-0.0144760874481498,
0.999273881220754));
#21149=DIRECTION('ref_axis',(0.379936674734162,-0.925012498938229,9.94761553655057E-13));
#21150=DIRECTION('',(-0.0352444126515999,-0.0144761773059668,0.999273872202936));
#21151=DIRECTION('',(-0.924544964574144,-0.381072970020941,1.15083568972965E-7));
#21152=DIRECTION('',(0.0352525125757934,0.0144550288485472,-0.999273892633087));
#21153=DIRECTION('center_axis',(0.0370212898762763,-0.0090044481677379,
0.99927390840004));
#21154=DIRECTION('ref_axis',(0.236333478441325,0.971672005857853,0.));
#21155=DIRECTION('',(-0.0370157050058834,0.00902614240225516,-0.999273919571732));
#21156=DIRECTION('center_axis',(-0.0370208532576561,0.009004341971824,-0.999273925532799));
#21157=DIRECTION('ref_axis',(0.970966499624253,-0.236161882735454,-0.0381001542027123));
#21158=DIRECTION('',(0.0370215148147411,-0.00900450287806193,0.999273899573456));
#21159=DIRECTION('',(0.972014875666751,-0.234919308449784,1.61392065502938E-7));
#21160=DIRECTION('center_axis',(0.,0.,-1.));
#21161=DIRECTION('ref_axis',(0.236333478439934,0.971672005858191,0.));
#21162=DIRECTION('',(0.,0.,1.));
#21163=DIRECTION('center_axis',(0.,0.,-1.));
#21164=DIRECTION('ref_axis',(0.236333478439934,0.971672005858191,0.));
#21165=DIRECTION('',(0.,0.,-1.));
#21166=DIRECTION('center_axis',(0.,0.,-1.));
#21167=DIRECTION('ref_axis',(-0.403523989416176,-0.914969065032066,0.));
#21168=DIRECTION('center_axis',(0.,0.,-1.));
#21169=DIRECTION('ref_axis',(0.236333478439908,0.971672005858198,0.));
#21170=DIRECTION('',(0.,0.,-1.));
#21171=DIRECTION('',(0.,0.,1.));
#21172=DIRECTION('center_axis',(0.,0.,-1.));
#21173=DIRECTION('ref_axis',(0.236333478439911,0.971672005858197,0.));
#21174=DIRECTION('center_axis',(0.,0.,1.));
#21175=DIRECTION('ref_axis',(0.236333478439923,0.971672005858194,0.));
#21176=DIRECTION('center_axis',(0.,0.,-1.));
#21177=DIRECTION('ref_axis',(0.236333478439911,0.971672005858197,0.));
#21178=DIRECTION('center_axis',(-0.23633347843992,-0.971672005858195,0.));
#21179=DIRECTION('ref_axis',(0.,0.,1.));
#21180=DIRECTION('center_axis',(0.276303824482695,0.961070339036762,1.44037777350484E-15));
#21181=DIRECTION('ref_axis',(-0.961070339036762,0.276303824482695,1.44348006936188E-29));
#21182=DIRECTION('center_axis',(-0.97167200585819,0.236333478439938,0.));
#21183=DIRECTION('ref_axis',(-0.236333478439938,-0.97167200585819,0.));
#21184=DIRECTION('center_axis',(0.,0.,-1.));
#21185=DIRECTION('ref_axis',(0.236333478439911,0.971672005858197,0.));
#21186=DIRECTION('center_axis',(0.,0.,1.));
#21187=DIRECTION('ref_axis',(0.236333478439911,0.971672005858197,0.));
#21188=DIRECTION('center_axis',(0.,0.,-1.));
#21189=DIRECTION('ref_axis',(0.236333478439911,0.971672005858197,0.));
#21190=DIRECTION('center_axis',(0.0352433370446482,0.0144757355146047,-0.999273916539038));
#21191=DIRECTION('ref_axis',(-0.379936674702656,0.92501249895117,2.84217572986559E-13));
#21192=DIRECTION('center_axis',(0.0352424754478559,0.0144753816250977,-0.999273952052747));
#21193=DIRECTION('ref_axis',(0.97121008913075,-0.23622112943089,0.0308308413935825));
#21194=DIRECTION('',(-0.0352341919267929,-0.0144959347334989,0.999273946220689));
#21195=DIRECTION('',(0.925650075050678,0.378380679420379,-2.15610283786586E-7));
#21196=DIRECTION('',(0.0352430917530489,0.0144756347643183,-0.999273926649673));
#21197=DIRECTION('center_axis',(0.,0.,-1.));
#21198=DIRECTION('ref_axis',(0.236333478439912,0.971672005858197,0.));
#21199=DIRECTION('center_axis',(0.,0.,-1.));
#21200=DIRECTION('ref_axis',(0.236333478439911,0.971672005858197,0.));
#21201=DIRECTION('center_axis',(0.971672005858197,-0.236333478439911,0.));
#21202=DIRECTION('ref_axis',(0.236333478439911,0.971672005858197,0.));
#21203=DIRECTION('',(-0.971672005858197,0.236333478439911,0.));
#21204=DIRECTION('',(0.971672005858197,-0.236333478439911,0.));
#21205=DIRECTION('center_axis',(0.,0.,-1.));
#21206=DIRECTION('ref_axis',(0.236333478439911,0.971672005858197,0.));
#21207=DIRECTION('center_axis',(0.993477056368512,0.114032181726723,-4.79607696935732E-15));
#21208=DIRECTION('ref_axis',(0.114032181726723,-0.993477056368512,3.69174078276775E-29));
#21209=DIRECTION('center_axis',(0.,0.,-1.));
#21210=DIRECTION('ref_axis',(0.236333478439911,0.971672005858197,0.));
#21211=DIRECTION('center_axis',(0.,0.,1.));
#21212=DIRECTION('ref_axis',(0.236333478439912,0.971672005858197,0.));
#21213=DIRECTION('center_axis',(0.,0.,-1.));
#21214=DIRECTION('ref_axis',(0.236333478439908,0.971672005858198,0.));
#21215=DIRECTION('',(0.,0.,1.));
#21216=DIRECTION('center_axis',(0.,0.,-1.));
#21217=DIRECTION('ref_axis',(0.236333478439908,0.971672005858198,0.));
#21218=DIRECTION('',(0.,0.,-1.));
#21219=DIRECTION('center_axis',(0.,0.,1.));
#21220=DIRECTION('ref_axis',(1.,0.,0.));
#21221=DIRECTION('center_axis',(-0.41745153963428,0.908699186781285,0.));
#21222=DIRECTION('ref_axis',(-0.908699186781285,-0.41745153963428,0.));
#21223=DIRECTION('center_axis',(0.925012498947636,0.37993667471126,-2.49982082791546E-14));
#21224=DIRECTION('ref_axis',(-0.37993667471126,0.925012498947636,3.50802986436712E-28));
#21225=DIRECTION('center_axis',(1.,0.,0.));
#21226=DIRECTION('ref_axis',(0.,-1.,0.));
#21227=DIRECTION('center_axis',(0.,0.,1.));
#21228=DIRECTION('ref_axis',(-0.236333478439928,-0.971672005858193,0.));
#21229=DIRECTION('center_axis',(0.0754966680795893,-0.997146054050699,0.));
#21230=DIRECTION('ref_axis',(0.997146054050699,0.0754966680795893,0.));
#21231=DIRECTION('center_axis',(0.925012498947636,0.37993667471126,0.));
#21232=DIRECTION('ref_axis',(-0.37993667471126,0.925012498947636,0.));
#21233=DIRECTION('',(-0.925012498947636,-0.379936674711261,0.));
#21234=DIRECTION('',(0.925012498947636,0.379936674711261,0.));
#21235=DIRECTION('center_axis',(0.,0.,-1.));
#21236=DIRECTION('ref_axis',(-0.525335493488004,-0.850895187012898,0.));
#21237=DIRECTION('center_axis',(0.,0.,-1.));
#21238=DIRECTION('ref_axis',(0.236333478439911,0.971672005858197,0.));
#21239=DIRECTION('center_axis',(-0.99942413970229,-0.0339321231333568,-6.28874166431797E-15));
#21240=DIRECTION('ref_axis',(-0.0339321231333568,0.99942413970229,-3.82846242175198E-29));
#21241=DIRECTION('center_axis',(-0.00287647308046481,0.0379919254018759,
-0.999273906147296));
#21242=DIRECTION('ref_axis',(-0.997146054050261,-0.0754966680853753,-2.84217577056821E-13));
#21243=DIRECTION('',(0.00289860077403835,-0.0379894563395136,0.99927393607588));
#21244=DIRECTION('',(-0.0739060517243553,0.997265208216189,-1.94028037262086E-7));
#21245=DIRECTION('',(-0.0028764528937826,0.0379916587798979,-0.999273916342212));
#21246=DIRECTION('center_axis',(-0.0754966680796036,0.997146054050698,0.));
#21247=DIRECTION('ref_axis',(-0.997146054050698,-0.0754966680796036,0.));
#21248=DIRECTION('',(-0.0754966680795988,0.997146054050699,0.));
#21249=DIRECTION('',(0.0754966680795988,-0.997146054050699,0.));
#21250=DIRECTION('center_axis',(0.,0.,-1.));
#21251=DIRECTION('ref_axis',(-0.636902289361219,-0.770944533547283,0.));
#21252=DIRECTION('',(0.,0.,-1.));
#21253=DIRECTION('',(0.,0.,1.));
#21254=DIRECTION('center_axis',(0.,0.,-1.));
#21255=DIRECTION('ref_axis',(0.236333478439928,0.971672005858193,0.));
#21256=DIRECTION('center_axis',(0.,0.,-1.));
#21257=DIRECTION('ref_axis',(-0.525317843056466,-0.850906083987242,0.));
#21258=DIRECTION('center_axis',(0.,0.,1.));
#21259=DIRECTION('ref_axis',(0.236333478439911,0.971672005858197,0.));
#21260=DIRECTION('center_axis',(0.,0.,-1.));
#21261=DIRECTION('ref_axis',(0.236333478439911,0.971672005858197,0.));
#21262=DIRECTION('center_axis',(0.,0.,-1.));
#21263=DIRECTION('ref_axis',(0.236333478439911,0.971672005858197,0.));
#21264=DIRECTION('center_axis',(0.,0.,1.));
#21265=DIRECTION('ref_axis',(1.,0.,0.));
#21266=DIRECTION('center_axis',(-0.0754966680795893,0.997146054050699,0.));
#21267=DIRECTION('ref_axis',(-0.997146054050699,-0.0754966680795893,0.));
#21268=DIRECTION('center_axis',(0.00287646743495555,-0.0379918508369929,
0.999273908998466));
#21269=DIRECTION('ref_axis',(-0.236178248992025,-0.971033788581598,-0.036238324132465));
#21270=DIRECTION('center_axis',(0.,0.,-1.));
#21271=DIRECTION('ref_axis',(0.236333478439911,0.971672005858197,0.));
#21272=DIRECTION('center_axis',(0.,0.,-1.));
#21273=DIRECTION('ref_axis',(0.236333478439911,0.971672005858197,0.));
#21274=DIRECTION('center_axis',(0.,0.,1.));
#21275=DIRECTION('ref_axis',(0.236333478439911,0.971672005858197,0.));
#21276=DIRECTION('center_axis',(0.,0.,-1.));
#21277=DIRECTION('ref_axis',(0.236333478439911,0.971672005858197,0.));
#21278=DIRECTION('center_axis',(0.,0.,-1.));
#21279=DIRECTION('ref_axis',(0.236333478439911,0.971672005858197,0.));
#21280=DIRECTION('center_axis',(0.,0.,1.));
#21281=DIRECTION('ref_axis',(0.236333478439911,0.971672005858197,0.));
#21282=DIRECTION('center_axis',(0.0754966680796036,-0.997146054050698,0.));
#21283=DIRECTION('ref_axis',(0.997146054050698,0.0754966680796036,0.));
#21284=DIRECTION('',(0.0754966680795988,-0.997146054050699,0.));
#21285=DIRECTION('',(-0.0754966680795988,0.997146054050699,0.));
#21286=DIRECTION('center_axis',(0.00287650181214345,-0.0379923048845794,
0.999273891636763));
#21287=DIRECTION('ref_axis',(0.997146054051204,0.0754966680729282,-2.84217582707585E-13));
#21288=DIRECTION('',(-0.00285399505219986,0.0379937044978036,-0.99927390295693));
#21289=DIRECTION('',(0.0028765195225703,-0.0379925388006534,0.999273882692286));
#21290=DIRECTION('',(0.0768080558201112,-0.997045897921012,1.31953752638336E-7));
#21291=DIRECTION('center_axis',(0.,0.,-1.));
#21292=DIRECTION('ref_axis',(0.236333478439928,0.971672005858193,0.));
#21293=DIRECTION('center_axis',(0.,0.,-1.));
#21294=DIRECTION('ref_axis',(0.236333478439928,0.971672005858193,0.));
#21295=DIRECTION('',(0.,0.,-1.));
#21296=DIRECTION('',(0.,0.,1.));
#21297=DIRECTION('center_axis',(0.,0.,-1.));
#21298=DIRECTION('ref_axis',(0.236333478439911,0.971672005858197,0.));
#21299=DIRECTION('center_axis',(0.,0.,-1.));
#21300=DIRECTION('ref_axis',(0.236333478439911,0.971672005858197,0.));
#21301=DIRECTION('center_axis',(-0.971672005858197,0.236333478439911,0.));
#21302=DIRECTION('ref_axis',(-0.236333478439911,-0.971672005858197,0.));
#21303=DIRECTION('center_axis',(0.,0.,1.));
#21304=DIRECTION('ref_axis',(0.236333478439911,0.971672005858197,0.));
#21305=DIRECTION('center_axis',(0.,0.,-1.));
#21306=DIRECTION('ref_axis',(0.236333478439911,0.971672005858197,0.));
#21307=DIRECTION('',(-0.971672005858197,0.236333478439911,0.));
#21308=DIRECTION('',(0.971672005858197,-0.236333478439911,0.));
#21309=DIRECTION('center_axis',(-0.236333478439911,-0.971672005858197,0.));
#21310=DIRECTION('ref_axis',(0.,0.,-1.));
#21311=DIRECTION('center_axis',(0.236333478439911,0.971672005858197,0.));
#21312=DIRECTION('ref_axis',(-0.971672005858197,0.236333478439911,0.));
#21313=DIRECTION('center_axis',(0.,0.,-1.));
#21314=DIRECTION('ref_axis',(0.236333478439911,0.971672005858197,0.));
#21315=DIRECTION('',(-0.0754966680795988,0.997146054050699,0.));
#21316=DIRECTION('',(0.0754966680795988,-0.997146054050699,0.));
#21317=DIRECTION('center_axis',(0.997146054050699,0.0754966680795988,0.));
#21318=DIRECTION('ref_axis',(0.,0.,1.));
#21319=DIRECTION('center_axis',(-0.997146054050699,-0.0754966680795988,
0.));
#21320=DIRECTION('ref_axis',(0.0754966680795988,-0.997146054050699,0.));
#21321=DIRECTION('center_axis',(0.,0.,-1.));
#21322=DIRECTION('ref_axis',(0.236333478439911,0.971672005858197,0.));
#21323=DIRECTION('',(0.925012498947636,0.379936674711261,0.));
#21324=DIRECTION('',(-0.925012498947635,-0.379936674711261,0.));
#21325=DIRECTION('center_axis',(0.379936674711261,-0.925012498947636,0.));
#21326=DIRECTION('ref_axis',(0.,0.,-1.));
#21327=DIRECTION('center_axis',(-0.379936674711261,0.925012498947635,0.));
#21328=DIRECTION('ref_axis',(0.,0.,-1.));
#21329=DIRECTION('center_axis',(0.,0.,-1.));
#21330=DIRECTION('ref_axis',(0.236333478439911,0.971672005858197,0.));
#21331=DIRECTION('',(0.647185832447714,-0.762332275506527,0.));
#21332=DIRECTION('',(-0.647185832447714,0.762332275506527,0.));
#21333=DIRECTION('center_axis',(-0.762332275506527,-0.647185832447714,0.));
#21334=DIRECTION('ref_axis',(-0.647185832447714,0.762332275506527,0.));
#21335=DIRECTION('center_axis',(0.762332275506527,0.647185832447714,0.));
#21336=DIRECTION('ref_axis',(0.,0.,1.));
#21337=DIRECTION('center_axis',(0.,0.,-1.));
#21338=DIRECTION('ref_axis',(0.236333478439911,0.971672005858197,0.));
#21339=DIRECTION('',(-0.525029657457553,-0.851083931695343,0.));
#21340=DIRECTION('',(0.525029657457553,0.851083931695343,0.));
#21341=DIRECTION('center_axis',(-0.851083931695343,0.525029657457553,0.));
#21342=DIRECTION('ref_axis',(0.,0.,-1.));
#21343=DIRECTION('center_axis',(0.851083931695343,-0.525029657457553,0.));
#21344=DIRECTION('ref_axis',(0.,0.,-1.));
#21345=DIRECTION('center_axis',(0.,0.,1.));
#21346=DIRECTION('ref_axis',(0.971672005858197,-0.236333478439911,0.));
#21347=DIRECTION('center_axis',(0.,0.,-1.));
#21348=DIRECTION('ref_axis',(0.236333478439911,0.971672005858197,0.));
#21349=DIRECTION('center_axis',(0.,0.,-1.));
#21350=DIRECTION('ref_axis',(0.236333478439911,0.971672005858197,0.));
#21351=DIRECTION('center_axis',(0.,0.,-1.));
#21352=DIRECTION('ref_axis',(0.236333478439911,0.971672005858197,0.));
#21353=DIRECTION('center_axis',(-0.971672005858197,0.236333478439911,0.));
#21354=DIRECTION('ref_axis',(-0.236333478439911,-0.971672005858197,0.));
#21355=DIRECTION('center_axis',(0.,0.,-1.));
#21356=DIRECTION('ref_axis',(0.236333478439911,0.971672005858197,0.));
#21357=DIRECTION('',(0.,0.,-1.));
#21358=DIRECTION('center_axis',(0.,0.,1.));
#21359=DIRECTION('ref_axis',(-0.236333478439911,-0.971672005858197,0.));
#21360=DIRECTION('',(0.00899665431329341,0.0369892458754347,0.999275165257665));
#21361=DIRECTION('center_axis',(0.,0.,-1.));
#21362=DIRECTION('ref_axis',(0.236333478439911,0.971672005858197,0.));
#21363=DIRECTION('center_axis',(0.,0.,-1.));
#21364=DIRECTION('ref_axis',(0.236333478439911,0.971672005858197,0.));
#21365=DIRECTION('',(0.,0.,1.));
#21366=DIRECTION('center_axis',(0.,0.,-1.));
#21367=DIRECTION('ref_axis',(0.236333478439911,0.971672005858197,0.));
#21368=DIRECTION('center_axis',(0.,0.,-1.));
#21369=DIRECTION('ref_axis',(0.236333478439911,0.971672005858197,0.));
#21370=DIRECTION('',(0.,0.,1.));
#21371=DIRECTION('center_axis',(0.,0.,-1.));
#21372=DIRECTION('ref_axis',(0.236333478439911,0.971672005858197,0.));
#21373=DIRECTION('center_axis',(0.,0.,-1.));
#21374=DIRECTION('ref_axis',(0.236333478439911,0.971672005858197,0.));
#21375=DIRECTION('center_axis',(0.,0.,-1.));
#21376=DIRECTION('ref_axis',(0.236333478439911,0.971672005858197,0.));
#21377=DIRECTION('center_axis',(0.,0.,-1.));
#21378=DIRECTION('ref_axis',(0.236333478439911,0.971672005858197,0.));
#21379=DIRECTION('axis',(0.,0.,1.));
#21380=DIRECTION('refdir',(1.,0.,0.));
#21381=DIRECTION('center_axis',(0.,0.,1.));
#21382=DIRECTION('ref_axis',(1.,0.,0.));
#21383=DIRECTION('center_axis',(0.,0.,-1.));
#21384=DIRECTION('ref_axis',(1.,0.,0.));
#21385=DIRECTION('',(0.,0.,1.));
#21386=DIRECTION('center_axis',(0.,0.,1.));
#21387=DIRECTION('ref_axis',(1.,0.,0.));
#21388=DIRECTION('',(0.,0.,-1.));
#21389=DIRECTION('center_axis',(0.,0.,1.));
#21390=DIRECTION('ref_axis',(1.,0.,0.));
#21391=DIRECTION('center_axis',(0.,0.,-1.));
#21392=DIRECTION('ref_axis',(1.,0.,0.));
#21393=DIRECTION('',(0.,0.,1.));
#21394=DIRECTION('center_axis',(0.,0.,1.));
#21395=DIRECTION('ref_axis',(1.,0.,0.));
#21396=DIRECTION('',(0.,0.,-1.));
#21397=DIRECTION('center_axis',(0.,0.,1.));
#21398=DIRECTION('ref_axis',(1.,0.,0.));
#21399=DIRECTION('center_axis',(0.,0.,-1.));
#21400=DIRECTION('ref_axis',(1.,0.,0.));
#21401=DIRECTION('',(0.,0.,1.));
#21402=DIRECTION('center_axis',(0.,0.,1.));
#21403=DIRECTION('ref_axis',(1.,0.,0.));
#21404=DIRECTION('',(0.,0.,-1.));
#21405=DIRECTION('center_axis',(0.,0.,1.));
#21406=DIRECTION('ref_axis',(1.,0.,0.));
#21407=DIRECTION('center_axis',(0.,0.,-1.));
#21408=DIRECTION('ref_axis',(1.,0.,0.));
#21409=DIRECTION('',(0.,0.,1.));
#21410=DIRECTION('center_axis',(0.,0.,1.));
#21411=DIRECTION('ref_axis',(1.,0.,0.));
#21412=DIRECTION('',(0.,0.,-1.));
#21413=DIRECTION('center_axis',(0.,0.,1.));
#21414=DIRECTION('ref_axis',(1.,0.,0.));
#21415=DIRECTION('center_axis',(0.,0.,-1.));
#21416=DIRECTION('ref_axis',(1.,0.,0.));
#21417=DIRECTION('',(0.,0.,1.));
#21418=DIRECTION('center_axis',(0.,0.,1.));
#21419=DIRECTION('ref_axis',(1.,0.,0.));
#21420=DIRECTION('',(0.,0.,-1.));
#21421=DIRECTION('center_axis',(0.,0.,1.));
#21422=DIRECTION('ref_axis',(1.,0.,0.));
#21423=DIRECTION('center_axis',(0.,0.,-1.));
#21424=DIRECTION('ref_axis',(1.,6.93889390390722E-15,0.));
#21425=DIRECTION('',(0.,0.,1.));
#21426=DIRECTION('center_axis',(0.,0.,1.));
#21427=DIRECTION('ref_axis',(1.,0.,0.));
#21428=DIRECTION('',(0.,0.,-1.));
#21429=DIRECTION('center_axis',(0.,0.,1.));
#21430=DIRECTION('ref_axis',(1.,0.,0.));
#21431=DIRECTION('center_axis',(0.,0.,1.));
#21432=DIRECTION('ref_axis',(1.,0.,0.));
#21433=DIRECTION('center_axis',(0.,0.,1.));
#21434=DIRECTION('ref_axis',(1.,0.,0.));
#21435=DIRECTION('',(-0.707106781186554,-8.65956056235502E-17,0.707106781186541));
#21436=DIRECTION('center_axis',(0.,0.,-1.));
#21437=DIRECTION('ref_axis',(1.,0.,0.));
#21438=DIRECTION('center_axis',(0.,0.,1.));
#21439=DIRECTION('ref_axis',(1.,0.,0.));
#21440=DIRECTION('center_axis',(0.,0.,1.));
#21441=DIRECTION('ref_axis',(1.,0.,0.));
#21442=DIRECTION('center_axis',(0.,0.,1.));
#21443=DIRECTION('ref_axis',(1.,0.,0.));
#21444=DIRECTION('',(-0.707106781186554,-8.65956056235501E-17,0.707106781186541));
#21445=DIRECTION('center_axis',(0.,0.,-1.));
#21446=DIRECTION('ref_axis',(1.,0.,0.));
#21447=DIRECTION('center_axis',(0.,0.,1.));
#21448=DIRECTION('ref_axis',(1.,0.,0.));
#21449=DIRECTION('center_axis',(0.,0.,1.));
#21450=DIRECTION('ref_axis',(1.,0.,0.));
#21451=DIRECTION('center_axis',(0.,0.,1.));
#21452=DIRECTION('ref_axis',(1.,0.,0.));
#21453=DIRECTION('',(-0.707106781186554,-8.65956056235502E-17,0.707106781186541));
#21454=DIRECTION('center_axis',(0.,0.,-1.));
#21455=DIRECTION('ref_axis',(1.,0.,0.));
#21456=DIRECTION('center_axis',(0.,0.,1.));
#21457=DIRECTION('ref_axis',(1.,0.,0.));
#21458=DIRECTION('center_axis',(0.,0.,1.));
#21459=DIRECTION('ref_axis',(1.,0.,0.));
#21460=DIRECTION('center_axis',(0.,0.,1.));
#21461=DIRECTION('ref_axis',(1.,0.,0.));
#21462=DIRECTION('',(-0.707106781186554,-8.65956056235501E-17,0.707106781186541));
#21463=DIRECTION('center_axis',(0.,0.,-1.));
#21464=DIRECTION('ref_axis',(1.,0.,0.));
#21465=DIRECTION('center_axis',(0.,0.,1.));
#21466=DIRECTION('ref_axis',(1.,0.,0.));
#21467=DIRECTION('center_axis',(0.,0.,1.));
#21468=DIRECTION('ref_axis',(1.,0.,0.));
#21469=DIRECTION('center_axis',(0.,0.,1.));
#21470=DIRECTION('ref_axis',(1.,0.,0.));
#21471=DIRECTION('',(-0.707106781186554,-8.65956056235501E-17,0.707106781186541));
#21472=DIRECTION('center_axis',(0.,0.,-1.));
#21473=DIRECTION('ref_axis',(1.,0.,0.));
#21474=DIRECTION('center_axis',(0.,0.,1.));
#21475=DIRECTION('ref_axis',(1.,0.,0.));
#21476=DIRECTION('center_axis',(0.,0.,1.));
#21477=DIRECTION('ref_axis',(1.,0.,0.));
#21478=DIRECTION('center_axis',(0.,0.,1.));
#21479=DIRECTION('ref_axis',(1.,0.,0.));
#21480=DIRECTION('',(-0.707106781186554,-8.65956056235501E-17,0.707106781186541));
#21481=DIRECTION('center_axis',(0.,0.,-1.));
#21482=DIRECTION('ref_axis',(1.,0.,0.));
#21483=DIRECTION('center_axis',(0.,0.,1.));
#21484=DIRECTION('ref_axis',(1.,0.,0.));
#21485=DIRECTION('center_axis',(0.,0.,1.));
#21486=DIRECTION('ref_axis',(1.,0.,0.));
#21487=DIRECTION('center_axis',(0.,0.,1.));
#21488=DIRECTION('ref_axis',(1.,0.,0.));
#21489=DIRECTION('',(-0.707106781186554,-8.65956056235501E-17,0.707106781186541));
#21490=DIRECTION('center_axis',(0.,0.,-1.));
#21491=DIRECTION('ref_axis',(1.,0.,0.));
#21492=DIRECTION('center_axis',(0.,0.,1.));
#21493=DIRECTION('ref_axis',(1.,0.,0.));
#21494=DIRECTION('center_axis',(0.,0.,1.));
#21495=DIRECTION('ref_axis',(1.,0.,0.));
#21496=DIRECTION('center_axis',(0.,0.,1.));
#21497=DIRECTION('ref_axis',(1.,0.,0.));
#21498=DIRECTION('',(-0.707106781186554,-8.65956056235501E-17,0.707106781186541));
#21499=DIRECTION('center_axis',(0.,0.,-1.));
#21500=DIRECTION('ref_axis',(1.,0.,0.));
#21501=DIRECTION('center_axis',(0.,0.,1.));
#21502=DIRECTION('ref_axis',(1.,0.,0.));
#21503=DIRECTION('center_axis',(0.,0.,1.));
#21504=DIRECTION('ref_axis',(1.,0.,0.));
#21505=DIRECTION('center_axis',(0.,0.,1.));
#21506=DIRECTION('ref_axis',(1.,0.,0.));
#21507=DIRECTION('',(-0.707106781186554,-8.65956056235501E-17,0.707106781186541));
#21508=DIRECTION('center_axis',(0.,0.,-1.));
#21509=DIRECTION('ref_axis',(1.,0.,0.));
#21510=DIRECTION('center_axis',(0.,0.,1.));
#21511=DIRECTION('ref_axis',(1.,0.,0.));
#21512=DIRECTION('center_axis',(0.,0.,1.));
#21513=DIRECTION('ref_axis',(1.,0.,0.));
#21514=DIRECTION('center_axis',(0.,0.,1.));
#21515=DIRECTION('ref_axis',(1.,0.,0.));
#21516=DIRECTION('',(-0.707106781186554,-8.65956056235501E-17,0.707106781186541));
#21517=DIRECTION('center_axis',(0.,0.,-1.));
#21518=DIRECTION('ref_axis',(1.,0.,0.));
#21519=DIRECTION('center_axis',(0.,0.,1.));
#21520=DIRECTION('ref_axis',(1.,0.,0.));
#21521=DIRECTION('center_axis',(0.,0.,1.));
#21522=DIRECTION('ref_axis',(1.,0.,0.));
#21523=DIRECTION('center_axis',(0.,0.,1.));
#21524=DIRECTION('ref_axis',(1.,0.,0.));
#21525=DIRECTION('',(-0.707106781186554,-8.65956056235502E-17,0.707106781186541));
#21526=DIRECTION('center_axis',(0.,0.,-1.));
#21527=DIRECTION('ref_axis',(1.,0.,0.));
#21528=DIRECTION('center_axis',(0.,0.,1.));
#21529=DIRECTION('ref_axis',(1.,0.,0.));
#21530=DIRECTION('center_axis',(0.,0.,1.));
#21531=DIRECTION('ref_axis',(1.,0.,0.));
#21532=DIRECTION('center_axis',(0.,0.,1.));
#21533=DIRECTION('ref_axis',(1.,0.,0.));
#21534=DIRECTION('',(-0.707106781186554,-8.65956056235502E-17,0.707106781186541));
#21535=DIRECTION('center_axis',(0.,0.,-1.));
#21536=DIRECTION('ref_axis',(1.,0.,0.));
#21537=DIRECTION('center_axis',(0.,0.,1.));
#21538=DIRECTION('ref_axis',(1.,0.,0.));
#21539=DIRECTION('center_axis',(0.,0.,1.));
#21540=DIRECTION('ref_axis',(1.,0.,0.));
#21541=DIRECTION('center_axis',(0.,0.,1.));
#21542=DIRECTION('ref_axis',(1.,0.,0.));
#21543=DIRECTION('',(-0.707106781186554,-8.65956056235501E-17,0.707106781186541));
#21544=DIRECTION('center_axis',(0.,0.,-1.));
#21545=DIRECTION('ref_axis',(1.,0.,0.));
#21546=DIRECTION('center_axis',(0.,0.,-1.));
#21547=DIRECTION('ref_axis',(0.,-1.,0.));
#21548=DIRECTION('',(0.,-1.,0.));
#21549=DIRECTION('',(1.,0.,0.));
#21550=DIRECTION('',(0.,1.,0.));
#21551=DIRECTION('',(-1.,0.,0.));
#21552=DIRECTION('center_axis',(1.,-4.08170229641602E-16,8.32946623846081E-32));
#21553=DIRECTION('ref_axis',(-4.08170229641602E-16,-1.,-4.19642196872632E-64));
#21554=DIRECTION('center_axis',(-1.,0.,-8.32946623846081E-32));
#21555=DIRECTION('ref_axis',(0.,1.,0.));
#21556=DIRECTION('',(-6.80579823082152E-36,-2.04085114820801E-16,-1.));
#21557=DIRECTION('',(-4.08170229641602E-16,-1.,0.));
#21558=DIRECTION('center_axis',(-1.,0.,-8.32946623846081E-32));
#21559=DIRECTION('ref_axis',(0.,1.,0.));
#21560=DIRECTION('',(-8.32946623846081E-32,-2.57814143119491E-47,1.));
#21561=DIRECTION('center_axis',(-1.,0.,-8.32946623846081E-32));
#21562=DIRECTION('ref_axis',(0.,1.,0.));
#21563=DIRECTION('',(4.08170229641602E-16,1.,-2.31296463463574E-16));
#21564=DIRECTION('',(-6.80579823082152E-36,-2.04085114820801E-16,-1.));
#21565=DIRECTION('',(-4.08170229641602E-16,-1.,2.04085114820801E-16));
#21566=DIRECTION('center_axis',(0.,2.14163392095902E-16,1.));
#21567=DIRECTION('ref_axis',(0.,-1.,2.14163392095902E-16));
#21568=DIRECTION('',(1.,3.0952060520883E-16,-7.15987345919025E-32));
#21569=DIRECTION('',(0.,-1.,2.14163392095902E-16));
#21570=DIRECTION('',(-1.,1.19262238973406E-16,0.));
#21571=DIRECTION('',(0.,1.,-2.14163392095902E-16));
#21572=DIRECTION('center_axis',(1.,-7.28776417516513E-52,-3.40289911541076E-36));
#21573=DIRECTION('ref_axis',(-3.40289911541076E-36,0.,-1.));
#21574=DIRECTION('',(0.,-1.,2.14163392095902E-16));
#21575=DIRECTION('',(-3.40289911541076E-36,-1.020425574104E-16,-1.));
#21576=DIRECTION('',(0.,-1.,2.14163392095902E-16));
#21577=DIRECTION('',(-3.40289911541076E-36,-1.020425574104E-16,-1.));
#21578=DIRECTION('center_axis',(-1.19262238973406E-16,-1.,1.020425574104E-16));
#21579=DIRECTION('ref_axis',(-1.,1.19262238973406E-16,0.));
#21580=DIRECTION('',(-1.,1.19262238973406E-16,0.));
#21581=DIRECTION('',(-3.40289911541076E-36,-1.020425574104E-16,-1.));
#21582=DIRECTION('center_axis',(-1.,7.28776417516513E-52,3.40289911541076E-36));
#21583=DIRECTION('ref_axis',(7.28776417516513E-52,1.,1.38699460815421E-104));
#21584=DIRECTION('',(0.,1.,-2.14163392095902E-16));
#21585=DIRECTION('',(-3.40289911541076E-36,-1.020425574104E-16,-1.));
#21586=DIRECTION('',(0.,1.,-2.14163392095902E-16));
#21587=DIRECTION('center_axis',(1.,0.,0.));
#21588=DIRECTION('ref_axis',(0.,1.,0.));
#21589=DIRECTION('',(1.,3.0952060520883E-16,0.));
#21590=DIRECTION('',(-1.,-3.0952060520883E-16,0.));
#21591=DIRECTION('center_axis',(-1.,0.,0.));
#21592=DIRECTION('ref_axis',(0.,-1.,0.));
#21593=DIRECTION('center_axis',(-1.,0.,7.15987345919025E-32));
#21594=DIRECTION('ref_axis',(0.,-1.,0.));
#21595=DIRECTION('',(1.,3.0952060520883E-16,-7.15987345919025E-32));
#21596=DIRECTION('',(-1.,-3.0952060520883E-16,7.15987345919025E-32));
#21597=DIRECTION('center_axis',(-1.,0.,0.));
#21598=DIRECTION('ref_axis',(0.,1.,0.));
#21599=DIRECTION('',(1.,3.0952060520883E-16,-7.15987345919025E-32));
#21600=DIRECTION('center_axis',(-1.,0.,0.));
#21601=DIRECTION('ref_axis',(0.,0.,1.));
#21602=DIRECTION('center_axis',(-1.,7.46735853138638E-19,0.));
#21603=DIRECTION('ref_axis',(7.46735853138638E-19,1.,0.));
#21604=DIRECTION('',(-1.,0.,0.));
#21605=DIRECTION('center_axis',(1.,0.,0.));
#21606=DIRECTION('ref_axis',(0.,0.,1.));
#21607=DIRECTION('',(1.,0.,0.));
#21608=DIRECTION('center_axis',(1.,0.,0.));
#21609=DIRECTION('ref_axis',(0.,0.,-1.));
#21610=DIRECTION('',(-1.,0.,6.80579823082152E-36));
#21611=DIRECTION('',(-1.,0.,6.80579823082152E-36));
#21612=DIRECTION('center_axis',(1.,0.,0.));
#21613=DIRECTION('ref_axis',(0.,1.,0.));
#21614=DIRECTION('',(1.,0.,-6.80579823082152E-36));
#21615=DIRECTION('center_axis',(1.,-3.33478423293997E-20,0.));
#21616=DIRECTION('ref_axis',(-3.33478423293997E-20,-1.,0.));
#21617=DIRECTION('',(6.42769832910921E-36,1.92747052886312E-16,1.));
#21618=DIRECTION('',(-3.33478423293997E-20,-1.,2.04085114820801E-16));
#21619=DIRECTION('',(0.,0.,-1.));
#21620=DIRECTION('',(3.33478423293997E-20,1.,-2.31296463463574E-16));
#21621=DIRECTION('',(-8.08152366190323E-36,-2.43945488809238E-16,-1.));
#21622=DIRECTION('',(3.33478423293997E-20,1.,0.));
#21623=DIRECTION('center_axis',(7.71323799493105E-36,2.31296463463574E-16,
1.));
#21624=DIRECTION('ref_axis',(0.,-1.,2.31296463463574E-16));
#21625=DIRECTION('',(-1.,3.33478423293997E-20,0.));
#21626=DIRECTION('center_axis',(3.33478423293997E-20,1.,0.));
#21627=DIRECTION('ref_axis',(1.,-3.33478423293997E-20,0.));
#21628=DIRECTION('',(-1.,3.33478423293997E-20,0.));
#21629=DIRECTION('center_axis',(-6.80579823082151E-36,-2.04085114820801E-16,
-1.));
#21630=DIRECTION('ref_axis',(0.,-1.,2.04085114820801E-16));
#21631=DIRECTION('center_axis',(0.,-1.,0.));
#21632=DIRECTION('ref_axis',(0.,0.,-1.));
#21633=DIRECTION('',(-1.,0.,0.));
#21634=DIRECTION('',(-1.,0.,0.));
#21635=DIRECTION('center_axis',(-1.,0.,0.));
#21636=DIRECTION('ref_axis',(0.,0.,1.));
#21637=DIRECTION('',(0.,1.,0.));
#21638=DIRECTION('',(0.,1.,0.));
#21639=DIRECTION('center_axis',(0.,1.,0.));
#21640=DIRECTION('ref_axis',(1.,0.,0.));
#21641=DIRECTION('',(1.,0.,0.));
#21642=DIRECTION('',(1.,0.,0.));
#21643=DIRECTION('center_axis',(1.,0.,0.));
#21644=DIRECTION('ref_axis',(0.,1.,0.));
#21645=DIRECTION('',(0.,-1.,0.));
#21646=DIRECTION('',(0.,-1.,0.));
#21647=DIRECTION('center_axis',(0.,0.,-1.));
#21648=DIRECTION('ref_axis',(-1.,0.,0.));
#21649=DIRECTION('',(0.,0.,-1.));
#21650=DIRECTION('center_axis',(0.,0.,1.));
#21651=DIRECTION('ref_axis',(1.,0.,0.));
#21652=DIRECTION('center_axis',(0.,0.,-1.));
#21653=DIRECTION('ref_axis',(-1.,0.,0.));
#21654=DIRECTION('center_axis',(0.,0.,1.));
#21655=DIRECTION('ref_axis',(1.,0.,0.));
#21656=DIRECTION('',(0.,0.,-1.));
#21657=DIRECTION('center_axis',(0.,0.,1.));
#21658=DIRECTION('ref_axis',(1.,0.,0.));
#21659=DIRECTION('center_axis',(0.,0.,-1.));
#21660=DIRECTION('ref_axis',(-1.,0.,0.));
#21661=DIRECTION('',(0.,0.,-1.));
#21662=DIRECTION('center_axis',(0.,0.,1.));
#21663=DIRECTION('ref_axis',(1.,0.,0.));
#21664=DIRECTION('center_axis',(0.,0.,-1.));
#21665=DIRECTION('ref_axis',(-1.,0.,0.));
#21666=DIRECTION('',(0.,0.,-1.));
#21667=DIRECTION('center_axis',(0.,0.,1.));
#21668=DIRECTION('ref_axis',(1.,0.,0.));
#21669=DIRECTION('center_axis',(0.,0.,-1.));
#21670=DIRECTION('ref_axis',(-1.,0.,0.));
#21671=DIRECTION('',(0.,0.,-1.));
#21672=DIRECTION('center_axis',(0.,0.,1.));
#21673=DIRECTION('ref_axis',(1.,0.,0.));
#21674=DIRECTION('center_axis',(0.,0.,-1.));
#21675=DIRECTION('ref_axis',(-1.,0.,0.));
#21676=DIRECTION('center_axis',(0.,0.,1.));
#21677=DIRECTION('ref_axis',(1.,0.,0.));
#21678=DIRECTION('',(0.,0.,-1.));
#21679=DIRECTION('center_axis',(0.,0.,1.));
#21680=DIRECTION('ref_axis',(1.,0.,0.));
#21681=DIRECTION('center_axis',(0.,0.,-1.));
#21682=DIRECTION('ref_axis',(-1.,0.,0.));
#21683=DIRECTION('center_axis',(0.,0.,1.));
#21684=DIRECTION('ref_axis',(1.,0.,0.));
#21685=DIRECTION('',(0.,0.,-1.));
#21686=DIRECTION('center_axis',(0.,0.,1.));
#21687=DIRECTION('ref_axis',(1.,0.,0.));
#21688=DIRECTION('center_axis',(0.,0.,-1.));
#21689=DIRECTION('ref_axis',(-1.,0.,0.));
#21690=DIRECTION('',(0.,0.,-1.));
#21691=DIRECTION('center_axis',(0.,0.,1.));
#21692=DIRECTION('ref_axis',(1.,0.,0.));
#21693=DIRECTION('center_axis',(0.,0.,-1.));
#21694=DIRECTION('ref_axis',(-1.,0.,0.));
#21695=DIRECTION('',(0.,0.,-1.));
#21696=DIRECTION('center_axis',(0.,0.,1.));
#21697=DIRECTION('ref_axis',(1.,0.,0.));
#21698=DIRECTION('center_axis',(0.,0.,-1.));
#21699=DIRECTION('ref_axis',(-1.,0.,0.));
#21700=DIRECTION('',(0.,0.,-1.));
#21701=DIRECTION('center_axis',(0.,0.,1.));
#21702=DIRECTION('ref_axis',(1.,0.,0.));
#21703=DIRECTION('center_axis',(0.,0.,-1.));
#21704=DIRECTION('ref_axis',(-1.,0.,0.));
#21705=DIRECTION('',(0.,0.,-1.));
#21706=DIRECTION('center_axis',(0.,0.,1.));
#21707=DIRECTION('ref_axis',(1.,0.,0.));
#21708=DIRECTION('center_axis',(0.,0.,-1.));
#21709=DIRECTION('ref_axis',(-1.,0.,0.));
#21710=DIRECTION('',(0.,0.,-1.));
#21711=DIRECTION('center_axis',(0.,0.,1.));
#21712=DIRECTION('ref_axis',(1.,0.,0.));
#21713=DIRECTION('center_axis',(0.,0.,-1.));
#21714=DIRECTION('ref_axis',(-1.,0.,0.));
#21715=DIRECTION('',(0.,0.,-1.));
#21716=DIRECTION('center_axis',(0.,0.,1.));
#21717=DIRECTION('ref_axis',(1.,0.,0.));
#21718=DIRECTION('center_axis',(0.,0.,-1.));
#21719=DIRECTION('ref_axis',(-1.,0.,0.));
#21720=DIRECTION('',(0.,0.,-1.));
#21721=DIRECTION('center_axis',(0.,0.,1.));
#21722=DIRECTION('ref_axis',(1.,0.,0.));
#21723=DIRECTION('center_axis',(0.,0.,-1.));
#21724=DIRECTION('ref_axis',(-1.,0.,0.));
#21725=DIRECTION('',(0.,0.,-1.));
#21726=DIRECTION('center_axis',(0.,0.,1.));
#21727=DIRECTION('ref_axis',(1.,0.,0.));
#21728=DIRECTION('center_axis',(0.,0.,-1.));
#21729=DIRECTION('ref_axis',(-1.,0.,0.));
#21730=DIRECTION('',(0.,0.,-1.));
#21731=DIRECTION('center_axis',(0.,0.,1.));
#21732=DIRECTION('ref_axis',(1.,0.,0.));
#21733=DIRECTION('center_axis',(0.,-1.,0.));
#21734=DIRECTION('ref_axis',(0.,0.,-1.));
#21735=DIRECTION('',(-1.,0.,0.));
#21736=DIRECTION('',(0.,0.,-1.));
#21737=DIRECTION('',(-1.,0.,0.));
#21738=DIRECTION('',(0.,0.,-1.));
#21739=DIRECTION('center_axis',(-1.,0.,0.));
#21740=DIRECTION('ref_axis',(0.,0.,1.));
#21741=DIRECTION('',(0.,1.,0.));
#21742=DIRECTION('',(0.,1.,0.));
#21743=DIRECTION('',(0.,0.,-1.));
#21744=DIRECTION('center_axis',(1.57296039774614E-16,-1.,0.));
#21745=DIRECTION('ref_axis',(0.,0.,-1.));
#21746=DIRECTION('',(-1.,-1.57296039774614E-16,0.));
#21747=DIRECTION('',(-1.,-1.57296039774614E-16,0.));
#21748=DIRECTION('center_axis',(0.968859201920176,-0.247612291404526,0.));
#21749=DIRECTION('ref_axis',(0.,0.,-1.));
#21750=DIRECTION('',(-0.247612291404526,-0.968859201920176,0.));
#21751=DIRECTION('',(-0.247612291404526,-0.968859201920176,0.));
#21752=DIRECTION('',(0.,0.,-1.));
#21753=DIRECTION('center_axis',(0.,0.,-1.));
#21754=DIRECTION('ref_axis',(-1.,0.,0.));
#21755=DIRECTION('center_axis',(0.,0.,1.));
#21756=DIRECTION('ref_axis',(1.,0.,0.));
#21757=DIRECTION('center_axis',(0.,0.,1.));
#21758=DIRECTION('ref_axis',(1.,0.,0.));
#21759=DIRECTION('',(0.,0.,-1.));
#21760=DIRECTION('center_axis',(5.33319398640883E-16,-1.,0.));
#21761=DIRECTION('ref_axis',(0.,0.,-1.));
#21762=DIRECTION('',(-1.,-5.33319398640883E-16,0.));
#21763=DIRECTION('',(-1.,-5.33319398640883E-16,0.));
#21764=DIRECTION('center_axis',(0.662145231497846,-0.74937553496539,0.));
#21765=DIRECTION('ref_axis',(0.,0.,-1.));
#21766=DIRECTION('',(-0.74937553496539,-0.662145231497846,0.));
#21767=DIRECTION('',(-0.74937553496539,-0.662145231497846,0.));
#21768=DIRECTION('',(0.,0.,-1.));
#21769=DIRECTION('center_axis',(0.,0.,-1.));
#21770=DIRECTION('ref_axis',(-1.,0.,0.));
#21771=DIRECTION('center_axis',(0.,0.,1.));
#21772=DIRECTION('ref_axis',(1.,0.,0.));
#21773=DIRECTION('center_axis',(0.,0.,1.));
#21774=DIRECTION('ref_axis',(1.,0.,0.));
#21775=DIRECTION('',(0.,0.,-1.));
#21776=DIRECTION('center_axis',(0.,-1.,0.));
#21777=DIRECTION('ref_axis',(0.,0.,-1.));
#21778=DIRECTION('',(-1.,0.,0.));
#21779=DIRECTION('',(-1.,0.,0.));
#21780=DIRECTION('',(0.,0.,-1.));
#21781=DIRECTION('center_axis',(0.,0.,-1.));
#21782=DIRECTION('ref_axis',(-1.,0.,0.));
#21783=DIRECTION('center_axis',(0.,0.,1.));
#21784=DIRECTION('ref_axis',(1.,0.,0.));
#21785=DIRECTION('center_axis',(0.,0.,1.));
#21786=DIRECTION('ref_axis',(1.,0.,0.));
#21787=DIRECTION('',(0.,0.,-1.));
#21788=DIRECTION('center_axis',(-1.,-2.0289026509807E-16,0.));
#21789=DIRECTION('ref_axis',(-2.0289026509807E-16,1.,0.));
#21790=DIRECTION('',(-2.0289026509807E-16,1.,0.));
#21791=DIRECTION('',(-2.0289026509807E-16,1.,0.));
#21792=DIRECTION('',(0.,0.,-1.));
#21793=DIRECTION('center_axis',(0.,1.,0.));
#21794=DIRECTION('ref_axis',(1.,0.,0.));
#21795=DIRECTION('',(0.,0.,-1.));
#21796=DIRECTION('',(0.,0.,-1.));
#21797=DIRECTION('',(-1.,-1.98254111540206E-16,0.));
#21798=DIRECTION('',(1.,0.,0.));
#21799=DIRECTION('',(1.,0.,0.));
#21800=DIRECTION('',(0.,0.,-1.));
#21801=DIRECTION('center_axis',(1.,0.,0.));
#21802=DIRECTION('ref_axis',(0.,1.,0.));
#21803=DIRECTION('',(0.,0.,-1.));
#21804=DIRECTION('',(0.,-1.,0.));
#21805=DIRECTION('center_axis',(3.0952060520883E-16,-1.,0.));
#21806=DIRECTION('ref_axis',(0.,0.,-1.));
#21807=DIRECTION('',(0.,0.,-1.));
#21808=DIRECTION('',(-1.,-3.0952060520883E-16,0.));
#21809=DIRECTION('',(0.,0.,-1.));
#21810=DIRECTION('',(-1.,3.33478423293997E-20,0.));
#21811=DIRECTION('',(0.,0.,-1.));
#21812=DIRECTION('',(-1.,-1.0842021724855E-16,0.));
#21813=DIRECTION('center_axis',(1.,3.75567552354677E-14,0.));
#21814=DIRECTION('ref_axis',(-3.75567552354678E-14,1.,0.));
#21815=DIRECTION('',(3.75567552354677E-14,-1.,0.));
#21816=DIRECTION('',(3.75567552354677E-14,-1.,0.));
#21817=DIRECTION('',(0.,0.,-1.));
#21818=DIRECTION('center_axis',(0.,1.,0.));
#21819=DIRECTION('ref_axis',(1.,0.,0.));
#21820=DIRECTION('',(1.,0.,0.));
#21821=DIRECTION('',(1.,0.,0.));
#21822=DIRECTION('',(0.,0.,-1.));
#21823=DIRECTION('center_axis',(-1.,-1.25189184118226E-14,0.));
#21824=DIRECTION('ref_axis',(-1.25189184118226E-14,1.,0.));
#21825=DIRECTION('',(-1.25189184118226E-14,1.,0.));
#21826=DIRECTION('',(-1.25189184118226E-14,1.,0.));
#21827=DIRECTION('center_axis',(-1.,0.,0.));
#21828=DIRECTION('ref_axis',(0.,0.,1.));
#21829=DIRECTION('',(0.,1.,0.));
#21830=DIRECTION('center_axis',(1.,-7.46735853138638E-19,0.));
#21831=DIRECTION('ref_axis',(-7.46735853138638E-19,-1.,0.));
#21832=DIRECTION('',(-7.46735853138638E-19,-1.,0.));
#21833=DIRECTION('',(-7.46735853138638E-19,-1.,0.));
#21834=DIRECTION('center_axis',(0.,0.,1.));
#21835=DIRECTION('ref_axis',(1.,0.,0.));
#21836=DIRECTION('center_axis',(0.,0.,1.));
#21837=DIRECTION('ref_axis',(1.,0.,0.));
#21838=DIRECTION('center_axis',(7.71323799493105E-36,2.31296463463574E-16,
1.));
#21839=DIRECTION('ref_axis',(0.,-1.,2.31296463463574E-16));
#21840=DIRECTION('',(-1.,3.33478423293997E-20,0.));
#21841=DIRECTION('center_axis',(3.33478423293997E-20,1.,0.));
#21842=DIRECTION('ref_axis',(1.,-3.33478423293997E-20,0.));
#21843=DIRECTION('',(-1.,3.33478423293997E-20,0.));
#21844=DIRECTION('center_axis',(-6.80579823082151E-36,-2.04085114820801E-16,
-1.));
#21845=DIRECTION('ref_axis',(0.,-1.,2.04085114820801E-16));
#21846=DIRECTION('axis',(0.,0.,1.));
#21847=DIRECTION('refdir',(1.,0.,0.));
#21848=DIRECTION('center_axis',(7.E-15,0.,1.));
#21849=DIRECTION('ref_axis',(-1.26181948956739E-14,-1.,8.76968602559222E-29));
#21850=DIRECTION('center_axis',(-7.E-15,0.,-1.));
#21851=DIRECTION('ref_axis',(-1.,0.,7.E-15));
#21852=DIRECTION('',(7.E-15,0.,1.));
#21853=DIRECTION('center_axis',(-7.E-15,0.,-1.));
#21854=DIRECTION('ref_axis',(-1.,0.,7.E-15));
#21855=DIRECTION('',(7.E-15,0.,1.));
#21856=DIRECTION('center_axis',(7.E-15,0.,1.));
#21857=DIRECTION('ref_axis',(-0.998223338976354,-0.0595832654601811,6.98756337283448E-15));
#21858=DIRECTION('center_axis',(7.E-15,0.,1.));
#21859=DIRECTION('ref_axis',(1.,0.,-7.E-15));
#21860=DIRECTION('',(7.E-15,0.,1.));
#21861=DIRECTION('center_axis',(7.E-15,0.,1.));
#21862=DIRECTION('ref_axis',(-1.,0.,7.E-15));
#21863=DIRECTION('',(-7.E-15,0.,-1.));
#21864=DIRECTION('center_axis',(-7.E-15,0.,-1.));
#21865=DIRECTION('ref_axis',(-1.,0.,7.E-15));
#21866=DIRECTION('',(0.,1.,0.));
#21867=DIRECTION('',(-1.,0.,7.E-15));
#21868=DIRECTION('',(1.,0.,-7.E-15));
#21869=DIRECTION('center_axis',(-1.,0.,7.E-15));
#21870=DIRECTION('ref_axis',(7.E-15,0.,1.));
#21871=DIRECTION('center_axis',(0.,-1.,0.));
#21872=DIRECTION('ref_axis',(-8.88178419700128E-15,0.,-1.));
#21873=DIRECTION('center_axis',(1.,0.,-7.E-15));
#21874=DIRECTION('ref_axis',(7.E-15,0.,1.));
#21875=DIRECTION('center_axis',(1.,0.,-7.E-15));
#21876=DIRECTION('ref_axis',(7.E-15,0.,1.));
#21877=DIRECTION('center_axis',(-1.,0.,7.E-15));
#21878=DIRECTION('ref_axis',(7.E-15,0.,1.));
#21879=DIRECTION('center_axis',(0.,-1.,0.));
#21880=DIRECTION('ref_axis',(-8.88178419700128E-15,0.,-1.));
#21881=DIRECTION('center_axis',(1.,0.,-7.E-15));
#21882=DIRECTION('ref_axis',(7.E-15,0.,1.));
#21883=DIRECTION('center_axis',(1.,0.,-7.E-15));
#21884=DIRECTION('ref_axis',(7.E-15,0.,1.));
#21885=DIRECTION('center_axis',(-1.,0.,7.E-15));
#21886=DIRECTION('ref_axis',(0.,1.,0.));
#21887=DIRECTION('center_axis',(1.,0.,-7.E-15));
#21888=DIRECTION('ref_axis',(-7.E-15,0.,-1.));
#21889=DIRECTION('center_axis',(-1.,0.,7.E-15));
#21890=DIRECTION('ref_axis',(-7.E-15,0.,-1.));
#21891=DIRECTION('',(-1.,0.,7.E-15));
#21892=DIRECTION('center_axis',(-1.,0.,7.E-15));
#21893=DIRECTION('ref_axis',(0.,1.,0.));
#21894=DIRECTION('center_axis',(1.,0.,-7.E-15));
#21895=DIRECTION('ref_axis',(-7.E-15,0.,-1.));
#21896=DIRECTION('center_axis',(-1.,0.,7.E-15));
#21897=DIRECTION('ref_axis',(-7.E-15,0.,-1.));
#21898=DIRECTION('',(-1.,0.,7.E-15));
#21899=DIRECTION('center_axis',(7.E-15,0.,1.));
#21900=DIRECTION('ref_axis',(0.,-1.,0.));
#21901=DIRECTION('',(1.,0.,-7.E-15));
#21902=DIRECTION('center_axis',(7.E-15,0.,1.));
#21903=DIRECTION('ref_axis',(0.,-1.,0.));
#21904=DIRECTION('',(0.,-1.,0.));
#21905=DIRECTION('',(-1.,0.,7.E-15));
#21906=DIRECTION('',(0.,1.,0.));
#21907=DIRECTION('',(1.,0.,-7.E-15));
#21908=DIRECTION('center_axis',(1.,0.,-7.E-15));
#21909=DIRECTION('ref_axis',(-7.E-15,0.,-1.));
#21910=DIRECTION('',(0.,1.,0.));
#21911=DIRECTION('',(7.E-15,0.,1.));
#21912=DIRECTION('',(7.E-15,0.,1.));
#21913=DIRECTION('center_axis',(0.,1.,0.));
#21914=DIRECTION('ref_axis',(-1.,0.,7.E-15));
#21915=DIRECTION('',(-1.,0.,7.E-15));
#21916=DIRECTION('',(7.E-15,0.,1.));
#21917=DIRECTION('center_axis',(-1.,0.,7.E-15));
#21918=DIRECTION('ref_axis',(0.,1.,0.));
#21919=DIRECTION('',(0.,-1.,0.));
#21920=DIRECTION('',(7.E-15,0.,1.));
#21921=DIRECTION('center_axis',(0.,-1.,0.));
#21922=DIRECTION('ref_axis',(7.E-15,0.,1.));
#21923=DIRECTION('',(1.,0.,-7.E-15));
#21924=DIRECTION('center_axis',(7.E-15,0.,1.));
#21925=DIRECTION('ref_axis',(0.,-1.,0.));
#21926=DIRECTION('axis',(0.,0.,1.));
#21927=DIRECTION('refdir',(1.,0.,0.));
#21928=DIRECTION('center_axis',(-0.332226829439148,0.943199519614387,0.));
#21929=DIRECTION('ref_axis',(0.,0.,-1.));
#21930=DIRECTION('',(-0.943199519614387,-0.332226829439149,0.));
#21931=DIRECTION('',(0.,0.,1.));
#21932=DIRECTION('',(-0.943199519614387,-0.332226829439149,0.));
#21933=DIRECTION('',(0.,0.,1.));
#21934=DIRECTION('center_axis',(-0.219923546994498,0.975517110807063,0.));
#21935=DIRECTION('ref_axis',(0.,0.,-1.));
#21936=DIRECTION('',(-0.975517110807063,-0.219923546994498,0.));
#21937=DIRECTION('',(0.,0.,1.));
#21938=DIRECTION('',(-0.975517110807063,-0.219923546994498,0.));
#21939=DIRECTION('',(0.,0.,1.));
#21940=DIRECTION('center_axis',(1.,-1.E-15,0.));
#21941=DIRECTION('ref_axis',(-1.E-15,-1.,0.));
#21942=DIRECTION('center_axis',(-1.,1.E-15,0.));
#21943=DIRECTION('ref_axis',(-1.E-15,-1.,0.));
#21944=DIRECTION('',(-1.,1.E-15,0.));
#21945=DIRECTION('center_axis',(1.,-1.E-15,0.));
#21946=DIRECTION('ref_axis',(0.,0.,1.));
#21947=DIRECTION('',(1.,-1.E-15,0.));
#21948=DIRECTION('center_axis',(1.,-1.E-15,0.));
#21949=DIRECTION('ref_axis',(-1.E-15,-1.,0.));
#21950=DIRECTION('center_axis',(1.,-1.E-15,0.));
#21951=DIRECTION('ref_axis',(-1.E-15,-1.,0.));
#21952=DIRECTION('',(-1.,1.E-15,0.));
#21953=DIRECTION('center_axis',(-1.,1.E-15,0.));
#21954=DIRECTION('ref_axis',(0.,0.,1.));
#21955=DIRECTION('',(1.,-1.E-15,0.));
#21956=DIRECTION('center_axis',(1.,-1.E-15,0.));
#21957=DIRECTION('ref_axis',(-1.E-15,-1.,0.));
#21958=DIRECTION('center_axis',(1.,-1.E-15,0.));
#21959=DIRECTION('ref_axis',(0.,0.,1.));
#21960=DIRECTION('',(1.,-1.E-15,0.));
#21961=DIRECTION('center_axis',(-1.,1.E-15,0.));
#21962=DIRECTION('ref_axis',(-1.E-15,-1.,0.));
#21963=DIRECTION('',(-1.,1.E-15,0.));
#21964=DIRECTION('center_axis',(-1.,1.E-15,0.));
#21965=DIRECTION('ref_axis',(1.E-15,1.,0.));
#21966=DIRECTION('center_axis',(-1.,1.E-15,0.));
#21967=DIRECTION('ref_axis',(0.,0.,1.));
#21968=DIRECTION('',(1.,-1.E-15,0.));
#21969=DIRECTION('center_axis',(1.,-1.E-15,0.));
#21970=DIRECTION('ref_axis',(-1.E-15,-1.,0.));
#21971=DIRECTION('',(-1.,1.E-15,0.));
#21972=DIRECTION('center_axis',(1.E-15,1.,0.));
#21973=DIRECTION('ref_axis',(1.,-1.E-15,0.));
#21974=DIRECTION('',(0.,0.,1.));
#21975=DIRECTION('',(0.,0.,-1.));
#21976=DIRECTION('',(-1.,1.E-15,0.));
#21977=DIRECTION('center_axis',(0.,0.,1.));
#21978=DIRECTION('ref_axis',(-1.E-15,-1.,0.));
#21979=DIRECTION('',(1.E-15,1.,0.));
#21980=DIRECTION('',(1.E-15,1.,0.));
#21981=DIRECTION('center_axis',(-1.E-15,-1.,0.));
#21982=DIRECTION('ref_axis',(0.,0.,1.));
#21983=DIRECTION('',(0.,0.,1.));
#21984=DIRECTION('',(0.,0.,-1.));
#21985=DIRECTION('',(1.,-1.E-15,0.));
#21986=DIRECTION('center_axis',(0.,0.,-1.));
#21987=DIRECTION('ref_axis',(1.,-1.E-15,0.));
#21988=DIRECTION('',(1.E-15,1.,0.));
#21989=DIRECTION('',(1.E-15,1.,0.));
#21990=DIRECTION('center_axis',(-1.E-15,-1.,0.));
#21991=DIRECTION('ref_axis',(0.,0.,1.));
#21992=DIRECTION('',(1.,-1.E-15,0.));
#21993=DIRECTION('',(0.,0.,1.));
#21994=DIRECTION('',(0.,0.,1.));
#21995=DIRECTION('',(-0.707106781186547,7.07106781186548E-16,-0.707106781186547));
#21996=DIRECTION('',(-1.,1.E-15,-5.77559370956749E-17));
#21997=DIRECTION('',(-0.707106781186547,7.07106781186547E-16,0.707106781186548));
#21998=DIRECTION('',(-1.,1.E-15,0.));
#21999=DIRECTION('',(0.,0.,-1.));
#22000=DIRECTION('',(-1.,1.E-15,0.));
#22001=DIRECTION('center_axis',(-1.E-15,-1.,0.));
#22002=DIRECTION('ref_axis',(0.,0.,1.));
#22003=DIRECTION('',(0.,0.,1.));
#22004=DIRECTION('',(1.,-1.E-15,0.));
#22005=DIRECTION('',(1.,-1.E-15,0.));
#22006=DIRECTION('',(0.,0.,-1.));
#22007=DIRECTION('',(-1.,1.E-15,0.));
#22008=DIRECTION('',(-0.707106781186547,7.07106781186547E-16,0.707106781186548));
#22009=DIRECTION('',(-1.,1.E-15,-5.77559370956749E-17));
#22010=DIRECTION('',(-0.707106781186547,7.07106781186548E-16,-0.707106781186547));
#22011=DIRECTION('',(4.94384700890794E-16,-4.94384700890794E-31,-1.));
#22012=DIRECTION('center_axis',(-1.,1.E-15,-4.94384700890794E-16));
#22013=DIRECTION('ref_axis',(1.E-15,1.,-2.03147768281658E-47));
#22014=DIRECTION('',(-1.E-15,-1.,0.));
#22015=DIRECTION('',(-1.E-15,-1.,0.));
#22016=DIRECTION('center_axis',(-0.707106781186548,7.07106781186548E-16,
0.707106781186548));
#22017=DIRECTION('ref_axis',(-0.707106781186548,7.07106781186547E-16,-0.707106781186548));
#22018=DIRECTION('',(-1.E-15,-1.,0.));
#22019=DIRECTION('center_axis',(-5.77559370956749E-17,5.77559370956749E-32,
1.));
#22020=DIRECTION('ref_axis',(-1.,1.E-15,-5.77559370956749E-17));
#22021=DIRECTION('',(-1.E-15,-1.,0.));
#22022=DIRECTION('center_axis',(0.707106781186548,-7.07106781186548E-16,
0.707106781186547));
#22023=DIRECTION('ref_axis',(-1.E-15,-1.,4.22628099173863E-32));
#22024=DIRECTION('',(-1.E-15,-1.,0.));
#22025=DIRECTION('center_axis',(0.,0.,1.));
#22026=DIRECTION('ref_axis',(-1.E-15,-1.,0.));
#22027=DIRECTION('',(-1.E-15,-1.,0.));
#22028=DIRECTION('center_axis',(-1.,1.E-15,0.));
#22029=DIRECTION('ref_axis',(1.E-15,1.,0.));
#22030=DIRECTION('',(-1.E-15,-1.,0.));
#22031=DIRECTION('center_axis',(0.,0.,1.));
#22032=DIRECTION('ref_axis',(-1.E-15,-1.,0.));
#22033=DIRECTION('',(-1.E-15,-1.,0.));
#22034=DIRECTION('center_axis',(-1.,1.E-15,6.93889390390723E-15));
#22035=DIRECTION('ref_axis',(-6.93889390390723E-15,6.93889390390723E-30,
-1.));
#22036=DIRECTION('',(-1.E-15,-1.,0.));
#22037=DIRECTION('center_axis',(1.,-1.E-15,0.));
#22038=DIRECTION('ref_axis',(0.,0.,-1.));
#22039=DIRECTION('',(-1.E-15,-1.,0.));
#22040=DIRECTION('',(-1.E-15,-1.,0.));
#22041=DIRECTION('center_axis',(0.,0.,1.));
#22042=DIRECTION('ref_axis',(-1.E-15,-1.,0.));
#22043=DIRECTION('center_axis',(0.,0.,-1.));
#22044=DIRECTION('ref_axis',(1.,-1.E-15,0.));
#22045=DIRECTION('axis',(0.,0.,1.));
#22046=DIRECTION('refdir',(1.,0.,0.));
#22047=DIRECTION('center_axis',(7.09000435319733E-16,2.91501601757459E-15,
-1.));
#22048=DIRECTION('ref_axis',(0.236333478439908,0.971672005858198,3.E-15));
#22049=DIRECTION('',(7.09000435319733E-16,2.91501601757459E-15,-1.));
#22050=DIRECTION('',(-7.09000435319733E-16,-2.91501601757459E-15,1.));
#22051=DIRECTION('center_axis',(7.09000435319733E-16,2.91501601757459E-15,
-1.));
#22052=DIRECTION('ref_axis',(-0.236333478439908,-0.971672005858198,-3.E-15));
#22053=DIRECTION('center_axis',(7.09000435319733E-16,2.91501601757459E-15,
-1.));
#22054=DIRECTION('ref_axis',(0.236333478439908,0.971672005858198,3.E-15));
#22055=DIRECTION('',(7.09000435319733E-16,2.91501601757459E-15,-1.));
#22056=DIRECTION('center_axis',(7.09000435319733E-16,2.91501601757459E-15,
-1.));
#22057=DIRECTION('ref_axis',(0.236333478439908,0.971672005858198,3.E-15));
#22058=DIRECTION('',(7.09000435319733E-16,2.91501601757459E-15,-1.));
#22059=DIRECTION('center_axis',(7.09000435319733E-16,2.91501601757459E-15,
-1.));
#22060=DIRECTION('ref_axis',(0.236333478439908,0.971672005858198,3.E-15));
#22061=DIRECTION('',(7.09000435319733E-16,2.91501601757459E-15,-1.));
#22062=DIRECTION('center_axis',(7.09000435319733E-16,2.91501601757459E-15,
-1.));
#22063=DIRECTION('ref_axis',(0.236333478439908,0.971672005858198,3.E-15));
#22064=DIRECTION('',(7.09000435319733E-16,2.91501601757459E-15,-1.));
#22065=DIRECTION('center_axis',(7.09000435319733E-16,2.91501601757459E-15,
-1.));
#22066=DIRECTION('ref_axis',(0.236333478439908,0.971672005858198,3.E-15));
#22067=DIRECTION('',(7.09000435319733E-16,2.91501601757459E-15,-1.));
#22068=DIRECTION('center_axis',(7.09000435319733E-16,2.91501601757459E-15,
-1.));
#22069=DIRECTION('ref_axis',(0.236333478439908,0.971672005858198,3.E-15));
#22070=DIRECTION('',(7.09000435319733E-16,2.91501601757459E-15,-1.));
#22071=DIRECTION('center_axis',(7.09000435319733E-16,2.91501601757459E-15,
-1.));
#22072=DIRECTION('ref_axis',(0.236333478439908,0.971672005858198,3.E-15));
#22073=DIRECTION('',(7.09000435319733E-16,2.91501601757459E-15,-1.));
#22074=DIRECTION('center_axis',(7.09000435319733E-16,2.91501601757459E-15,
-1.));
#22075=DIRECTION('ref_axis',(0.236333478439908,0.971672005858198,3.E-15));
#22076=DIRECTION('',(7.09000435319733E-16,2.91501601757459E-15,-1.));
#22077=DIRECTION('center_axis',(7.09000435319733E-16,2.91501601757459E-15,
-1.));
#22078=DIRECTION('ref_axis',(0.236333478439908,0.971672005858198,3.E-15));
#22079=DIRECTION('',(7.09000435319733E-16,2.91501601757459E-15,-1.));
#22080=DIRECTION('center_axis',(7.09000435319733E-16,2.91501601757459E-15,
-1.));
#22081=DIRECTION('ref_axis',(0.236333478439908,0.971672005858198,3.E-15));
#22082=DIRECTION('',(7.09000435319733E-16,2.91501601757459E-15,-1.));
#22083=DIRECTION('center_axis',(7.09000435319733E-16,2.91501601757459E-15,
-1.));
#22084=DIRECTION('ref_axis',(0.236333478439908,0.971672005858198,3.E-15));
#22085=DIRECTION('',(7.09000435319733E-16,2.91501601757459E-15,-1.));
#22086=DIRECTION('center_axis',(7.09000435319733E-16,2.91501601757459E-15,
-1.));
#22087=DIRECTION('ref_axis',(0.236333478439908,0.971672005858198,3.E-15));
#22088=DIRECTION('',(7.09000435319733E-16,2.91501601757459E-15,-1.));
#22089=DIRECTION('center_axis',(7.09000435319733E-16,2.91501601757459E-15,
-1.));
#22090=DIRECTION('ref_axis',(0.236333478439908,0.971672005858198,3.E-15));
#22091=DIRECTION('',(7.09000435319733E-16,2.91501601757459E-15,-1.));
#22092=DIRECTION('center_axis',(7.09000435319733E-16,2.91501601757459E-15,
-1.));
#22093=DIRECTION('ref_axis',(0.236333478439908,0.971672005858198,3.E-15));
#22094=DIRECTION('',(7.09000435319733E-16,2.91501601757459E-15,-1.));
#22095=DIRECTION('center_axis',(7.09000435319733E-16,2.91501601757459E-15,
-1.));
#22096=DIRECTION('ref_axis',(0.236333478439908,0.971672005858198,3.E-15));
#22097=DIRECTION('',(7.09000435319733E-16,2.91501601757459E-15,-1.));
#22098=DIRECTION('center_axis',(7.09000435319733E-16,2.91501601757459E-15,
-1.));
#22099=DIRECTION('ref_axis',(0.236333478439908,0.971672005858198,3.E-15));
#22100=DIRECTION('',(7.09000435319733E-16,2.91501601757459E-15,-1.));
#22101=DIRECTION('center_axis',(7.09000435319733E-16,2.91501601757459E-15,
-1.));
#22102=DIRECTION('ref_axis',(0.236333478439908,0.971672005858198,3.E-15));
#22103=DIRECTION('',(7.09000435319733E-16,2.91501601757459E-15,-1.));
#22104=DIRECTION('center_axis',(7.09000435319733E-16,2.91501601757459E-15,
-1.));
#22105=DIRECTION('ref_axis',(0.236333478439908,0.971672005858198,3.E-15));
#22106=DIRECTION('',(7.09000435319733E-16,2.91501601757459E-15,-1.));
#22107=DIRECTION('center_axis',(-7.09000435319733E-16,-2.91501601757459E-15,
1.));
#22108=DIRECTION('ref_axis',(-0.236333478439908,-0.971672005858198,-3.E-15));
#22109=DIRECTION('center_axis',(-9.36335395655066E-14,2.27738783980021E-14,
1.));
#22110=DIRECTION('ref_axis',(-0.236333478439913,-0.971672005858196,0.));
#22111=DIRECTION('',(-9.36335395655066E-14,2.27738783980021E-14,1.));
#22112=DIRECTION('center_axis',(-7.09000435319733E-16,-2.91501601757459E-15,
1.));
#22113=DIRECTION('ref_axis',(-0.236333478439908,-0.971672005858198,-3.E-15));
#22114=DIRECTION('center_axis',(-0.0526028585739488,0.0502161354828127,
0.997352133906085));
#22115=DIRECTION('ref_axis',(0.721410631826286,-0.688678429526452,0.0727235930972822));
#22116=DIRECTION('',(7.09000435319733E-16,2.91501601757459E-15,-1.));
#22117=DIRECTION('center_axis',(0.,0.,1.));
#22118=DIRECTION('ref_axis',(-0.236333478439877,-0.971672005858205,0.));
#22119=DIRECTION('',(0.,0.,1.));
#22120=DIRECTION('',(-7.09000435319733E-16,-2.91501601757459E-15,1.));
#22121=DIRECTION('center_axis',(0.,0.,1.));
#22122=DIRECTION('ref_axis',(-0.236333478439877,-0.971672005858205,0.));
#22123=DIRECTION('',(0.,0.,1.));
#22124=DIRECTION('center_axis',(0.,0.,1.));
#22125=DIRECTION('ref_axis',(-0.236333478439877,-0.971672005858205,0.));
#22126=DIRECTION('',(0.,0.,1.));
#22127=DIRECTION('center_axis',(0.,0.,1.));
#22128=DIRECTION('ref_axis',(-0.236333478439877,-0.971672005858205,0.));
#22129=DIRECTION('',(0.,0.,1.));
#22130=DIRECTION('center_axis',(0.,0.,1.));
#22131=DIRECTION('ref_axis',(-0.236333478439877,-0.971672005858205,0.));
#22132=DIRECTION('',(0.,0.,1.));
#22133=DIRECTION('center_axis',(0.,0.,1.));
#22134=DIRECTION('ref_axis',(-0.236333478439877,-0.971672005858205,0.));
#22135=DIRECTION('',(0.,0.,1.));
#22136=DIRECTION('center_axis',(0.,0.,1.));
#22137=DIRECTION('ref_axis',(-0.236333478439877,-0.971672005858205,0.));
#22138=DIRECTION('',(0.,0.,1.));
#22139=DIRECTION('center_axis',(0.,0.,1.));
#22140=DIRECTION('ref_axis',(-0.236333478439877,-0.971672005858205,0.));
#22141=DIRECTION('',(0.,0.,1.));
#22142=DIRECTION('center_axis',(0.,0.,1.));
#22143=DIRECTION('ref_axis',(-0.236333478439877,-0.971672005858205,0.));
#22144=DIRECTION('',(0.,0.,1.));
#22145=DIRECTION('center_axis',(0.,0.,1.));
#22146=DIRECTION('ref_axis',(-0.236333478439877,-0.971672005858205,0.));
#22147=DIRECTION('',(0.,0.,1.));
#22148=DIRECTION('center_axis',(0.,0.,1.));
#22149=DIRECTION('ref_axis',(-0.236333478439877,-0.971672005858205,0.));
#22150=DIRECTION('',(0.,0.,1.));
#22151=DIRECTION('center_axis',(0.,0.,1.));
#22152=DIRECTION('ref_axis',(-0.236333478439877,-0.971672005858205,0.));
#22153=DIRECTION('',(0.,0.,1.));
#22154=DIRECTION('center_axis',(0.,0.,1.));
#22155=DIRECTION('ref_axis',(-0.236333478439877,-0.971672005858205,0.));
#22156=DIRECTION('',(0.,0.,1.));
#22157=DIRECTION('center_axis',(0.,0.,1.));
#22158=DIRECTION('ref_axis',(-0.236333478439877,-0.971672005858205,0.));
#22159=DIRECTION('',(0.,0.,1.));
#22160=DIRECTION('center_axis',(0.,0.,1.));
#22161=DIRECTION('ref_axis',(-0.236333478439877,-0.971672005858205,0.));
#22162=DIRECTION('',(0.,0.,1.));
#22163=DIRECTION('center_axis',(0.,0.,1.));
#22164=DIRECTION('ref_axis',(-0.236333478439877,-0.971672005858205,0.));
#22165=DIRECTION('',(0.,0.,1.));
#22166=DIRECTION('center_axis',(0.,0.,1.));
#22167=DIRECTION('ref_axis',(-0.236333478439877,-0.971672005858205,0.));
#22168=DIRECTION('',(0.,0.,1.));
#22169=DIRECTION('center_axis',(0.,0.,1.));
#22170=DIRECTION('ref_axis',(-0.236333478439877,-0.971672005858205,0.));
#22171=DIRECTION('',(0.,0.,1.));
#22172=DIRECTION('center_axis',(0.,0.,1.));
#22173=DIRECTION('ref_axis',(-0.236333478439877,-0.971672005858205,0.));
#22174=DIRECTION('',(0.,0.,1.));
#22175=DIRECTION('center_axis',(0.,0.,1.));
#22176=DIRECTION('ref_axis',(-0.236333478439877,-0.971672005858205,0.));
#22177=DIRECTION('',(0.,0.,1.));
#22178=DIRECTION('',(7.09000435319733E-16,2.91501601757459E-15,-1.));
#22179=DIRECTION('center_axis',(-7.09000435319733E-16,-2.91501601757459E-15,
1.));
#22180=DIRECTION('ref_axis',(-0.236333478439911,-0.971672005858197,-3.E-15));
#22181=DIRECTION('',(7.09000435319733E-16,2.91501601757459E-15,-1.));
#22182=DIRECTION('center_axis',(0.,0.,1.));
#22183=DIRECTION('ref_axis',(1.,0.,0.));
#22184=DIRECTION('center_axis',(-7.09000435319733E-16,-2.91501601757459E-15,
1.));
#22185=DIRECTION('ref_axis',(-0.236333478439911,-0.971672005858197,-3.E-15));
#22186=DIRECTION('',(7.09000435319733E-16,2.91501601757459E-15,-1.));
#22187=DIRECTION('center_axis',(-7.09000435319733E-16,-2.91501601757459E-15,
1.));
#22188=DIRECTION('ref_axis',(-0.236333478439911,-0.971672005858197,-3.E-15));
#22189=DIRECTION('',(7.09000435319733E-16,2.91501601757459E-15,-1.));
#22190=DIRECTION('center_axis',(0.,0.,-1.));
#22191=DIRECTION('ref_axis',(-0.236333478439914,-0.971672005858196,0.));
#22192=DIRECTION('',(0.,0.,1.));
#22193=DIRECTION('',(-7.09000435319733E-16,-2.91501601757459E-15,1.));
#22194=DIRECTION('center_axis',(0.,0.,-1.));
#22195=DIRECTION('ref_axis',(-0.236333478439914,-0.971672005858196,0.));
#22196=DIRECTION('',(0.,0.,1.));
#22197=DIRECTION('center_axis',(0.,0.,-1.));
#22198=DIRECTION('ref_axis',(-0.236333478439914,-0.971672005858196,0.));
#22199=DIRECTION('',(0.,0.,1.));
#22200=DIRECTION('center_axis',(0.,0.,-1.));
#22201=DIRECTION('ref_axis',(-0.236333478439914,-0.971672005858196,0.));
#22202=DIRECTION('',(0.,0.,1.));
#22203=DIRECTION('center_axis',(0.,0.,-1.));
#22204=DIRECTION('ref_axis',(-0.236333478439914,-0.971672005858196,0.));
#22205=DIRECTION('',(0.,0.,1.));
#22206=DIRECTION('center_axis',(0.,0.,-1.));
#22207=DIRECTION('ref_axis',(-0.236333478439914,-0.971672005858196,0.));
#22208=DIRECTION('',(0.,0.,1.));
#22209=DIRECTION('center_axis',(0.,0.,-1.));
#22210=DIRECTION('ref_axis',(-0.236333478439914,-0.971672005858196,0.));
#22211=DIRECTION('',(0.,0.,1.));
#22212=DIRECTION('center_axis',(0.,0.,-1.));
#22213=DIRECTION('ref_axis',(-0.236333478439914,-0.971672005858196,0.));
#22214=DIRECTION('',(0.,0.,1.));
#22215=DIRECTION('center_axis',(0.,0.,1.));
#22216=DIRECTION('ref_axis',(0.851485939575788,-0.524377435350471,0.));
#22217=DIRECTION('',(0.,0.,1.));
#22218=DIRECTION('center_axis',(0.,0.,1.));
#22219=DIRECTION('ref_axis',(0.851485939575788,-0.524377435350471,0.));
#22220=DIRECTION('center_axis',(0.,0.,1.));
#22221=DIRECTION('ref_axis',(0.851485939575788,-0.524377435350471,0.));
#22222=DIRECTION('',(0.,0.,1.));
#22223=DIRECTION('center_axis',(0.,0.,1.));
#22224=DIRECTION('ref_axis',(0.851485939575788,-0.524377435350471,0.));
#22225=DIRECTION('',(0.,0.,1.));
#22226=DIRECTION('center_axis',(0.,0.,1.));
#22227=DIRECTION('ref_axis',(0.851485939575788,-0.524377435350471,0.));
#22228=DIRECTION('',(0.,0.,1.));
#22229=DIRECTION('',(0.,0.,-1.));
#22230=DIRECTION('center_axis',(0.,0.,1.));
#22231=DIRECTION('ref_axis',(0.851485939575788,-0.524377435350471,0.));
#22232=DIRECTION('center_axis',(0.,0.,1.));
#22233=DIRECTION('ref_axis',(0.851485939575788,-0.524377435350472,0.));
#22234=DIRECTION('center_axis',(0.,0.,-1.));
#22235=DIRECTION('ref_axis',(0.85148593957579,-0.524377435350467,0.));
#22236=DIRECTION('',(0.524377435350472,0.851485939575788,0.));
#22237=DIRECTION('',(0.851485939575788,-0.524377435350471,0.));
#22238=DIRECTION('',(-0.524377435350472,-0.851485939575788,0.));
#22239=DIRECTION('center_axis',(-0.524377435350472,-0.851485939575788,0.));
#22240=DIRECTION('ref_axis',(-0.851485939575788,0.524377435350472,0.));
#22241=DIRECTION('',(0.,0.,1.));
#22242=DIRECTION('',(0.,0.,1.));
#22243=DIRECTION('center_axis',(0.851485939575788,-0.524377435350471,0.));
#22244=DIRECTION('ref_axis',(-0.524377435350472,-0.851485939575788,0.));
#22245=DIRECTION('',(0.524377435350472,0.851485939575788,0.));
#22246=DIRECTION('',(0.,0.,-1.));
#22247=DIRECTION('center_axis',(-0.851485939575788,0.524377435350471,0.));
#22248=DIRECTION('ref_axis',(-0.524377435350472,-0.851485939575788,0.));
#22249=DIRECTION('',(0.,0.,1.));
#22250=DIRECTION('',(-0.524377435350472,-0.851485939575788,0.));
#22251=DIRECTION('center_axis',(0.,0.,-1.));
#22252=DIRECTION('ref_axis',(0.524377435350472,0.851485939575788,0.));
#22253=DIRECTION('',(0.851485939575786,-0.524377435350475,0.));
#22254=DIRECTION('',(-0.524377435350475,-0.851485939575786,0.));
#22255=DIRECTION('',(-0.851485939575786,0.524377435350475,0.));
#22256=DIRECTION('center_axis',(0.,0.,1.));
#22257=DIRECTION('ref_axis',(-0.851485939575788,0.524377435350472,0.));
#22258=DIRECTION('center_axis',(0.524377435350475,0.851485939575786,0.));
#22259=DIRECTION('ref_axis',(-0.851485939575786,0.524377435350475,0.));
#22260=DIRECTION('',(0.,0.,1.));
#22261=DIRECTION('',(-0.851485939575786,0.524377435350475,0.));
#22262=DIRECTION('',(0.,0.,1.));
#22263=DIRECTION('center_axis',(-0.851485939575786,0.524377435350475,0.));
#22264=DIRECTION('ref_axis',(0.,0.,1.));
#22265=DIRECTION('',(0.,0.,1.));
#22266=DIRECTION('center_axis',(-0.524377435350475,-0.851485939575786,0.));
#22267=DIRECTION('ref_axis',(-0.851485939575786,0.524377435350475,0.));
#22268=DIRECTION('',(0.851485939575786,-0.524377435350475,0.));
#22269=DIRECTION('',(0.,0.,-1.));
#22270=DIRECTION('center_axis',(0.,0.,-1.));
#22271=DIRECTION('ref_axis',(0.524377435350472,0.851485939575788,0.));
#22272=DIRECTION('',(-0.524377435350471,-0.851485939575788,0.));
#22273=DIRECTION('',(-0.851485939575788,0.524377435350472,0.));
#22274=DIRECTION('',(0.524377435350472,0.851485939575788,0.));
#22275=DIRECTION('center_axis',(0.,0.,1.));
#22276=DIRECTION('ref_axis',(-0.851485939575788,0.524377435350472,0.));
#22277=DIRECTION('center_axis',(0.851485939575788,-0.524377435350471,0.));
#22278=DIRECTION('ref_axis',(-0.524377435350472,-0.851485939575788,0.));
#22279=DIRECTION('',(0.,0.,1.));
#22280=DIRECTION('',(0.524377435350472,0.851485939575788,0.));
#22281=DIRECTION('',(0.,0.,1.));
#22282=DIRECTION('center_axis',(0.524377435350472,0.851485939575788,0.));
#22283=DIRECTION('ref_axis',(0.,0.,-1.));
#22284=DIRECTION('',(0.,0.,1.));
#22285=DIRECTION('center_axis',(-0.851485939575788,0.524377435350471,0.));
#22286=DIRECTION('ref_axis',(-0.524377435350471,-0.851485939575788,0.));
#22287=DIRECTION('',(-0.524377435350471,-0.851485939575788,0.));
#22288=DIRECTION('',(0.,0.,-1.));
#22289=DIRECTION('center_axis',(0.,0.,-1.));
#22290=DIRECTION('ref_axis',(0.524377435350472,0.851485939575788,0.));
#22291=DIRECTION('',(-0.851485939575788,0.524377435350471,0.));
#22292=DIRECTION('',(0.524377435350472,0.851485939575788,0.));
#22293=DIRECTION('',(0.851485939575788,-0.524377435350471,0.));
#22294=DIRECTION('center_axis',(0.,0.,1.));
#22295=DIRECTION('ref_axis',(-0.851485939575788,0.524377435350472,0.));
#22296=DIRECTION('center_axis',(0.,0.,1.));
#22297=DIRECTION('ref_axis',(-0.851485939575788,0.524377435350472,0.));
#22298=DIRECTION('center_axis',(-0.524377435350471,-0.851485939575788,0.));
#22299=DIRECTION('ref_axis',(0.,0.,1.));
#22300=DIRECTION('',(0.,0.,1.));
#22301=DIRECTION('',(0.851485939575788,-0.524377435350471,0.));
#22302=DIRECTION('',(0.,0.,1.));
#22303=DIRECTION('center_axis',(0.851485939575788,-0.524377435350472,0.));
#22304=DIRECTION('ref_axis',(0.,0.,-1.));
#22305=DIRECTION('',(0.,0.,1.));
#22306=DIRECTION('center_axis',(0.524377435350471,0.851485939575788,0.));
#22307=DIRECTION('ref_axis',(-0.851485939575788,0.524377435350471,0.));
#22308=DIRECTION('',(-0.851485939575788,0.524377435350471,0.));
#22309=DIRECTION('',(0.,0.,-1.));
#22310=DIRECTION('center_axis',(0.,0.,1.));
#22311=DIRECTION('ref_axis',(0.851485939575788,-0.524377435350471,0.));
#22312=DIRECTION('center_axis',(0.,0.,1.));
#22313=DIRECTION('ref_axis',(0.851485939575788,-0.524377435350471,0.));
#22314=DIRECTION('center_axis',(0.,0.,1.));
#22315=DIRECTION('ref_axis',(0.851485939575788,-0.524377435350471,0.));
#22316=DIRECTION('center_axis',(0.,0.,1.));
#22317=DIRECTION('ref_axis',(0.851485939575788,-0.524377435350472,0.));
#22318=DIRECTION('center_axis',(0.,0.,1.));
#22319=DIRECTION('ref_axis',(0.851485939575788,-0.524377435350472,0.));
#22320=DIRECTION('center_axis',(0.,0.,1.));
#22321=DIRECTION('ref_axis',(0.851485939575788,-0.524377435350472,0.));
#22322=DIRECTION('center_axis',(0.,0.,1.));
#22323=DIRECTION('ref_axis',(0.851485939575788,-0.524377435350472,0.));
#22324=DIRECTION('',(0.,0.,-1.));
#22325=DIRECTION('center_axis',(0.,0.,1.));
#22326=DIRECTION('ref_axis',(0.851485939575788,-0.524377435350472,0.));
#22327=DIRECTION('center_axis',(0.,0.,1.));
#22328=DIRECTION('ref_axis',(0.851485939575788,-0.524377435350472,0.));
#22329=DIRECTION('center_axis',(0.,0.,1.));
#22330=DIRECTION('ref_axis',(0.851485939575788,-0.524377435350472,0.));
#22331=DIRECTION('center_axis',(0.,0.,1.));
#22332=DIRECTION('ref_axis',(0.851485939575788,-0.524377435350472,0.));
#22333=DIRECTION('center_axis',(0.,0.,1.));
#22334=DIRECTION('ref_axis',(0.851485939575788,-0.524377435350471,0.));
#22335=DIRECTION('center_axis',(0.,0.,1.));
#22336=DIRECTION('ref_axis',(0.851485939575788,-0.524377435350471,0.));
#22337=DIRECTION('',(0.,0.,1.));
#22338=DIRECTION('center_axis',(-7.09000435319733E-16,-2.91501601757459E-15,
1.));
#22339=DIRECTION('ref_axis',(3.62723386184346E-31,1.,2.91501601757459E-15));
#22340=DIRECTION('center_axis',(0.,0.,1.));
#22341=DIRECTION('ref_axis',(0.851485939575787,-0.524377435350472,0.));
#22342=DIRECTION('center_axis',(0.,0.,1.));
#22343=DIRECTION('ref_axis',(0.851485939575787,-0.524377435350472,0.));
#22344=DIRECTION('center_axis',(-0.524377435350472,-0.851485939575788,0.));
#22345=DIRECTION('ref_axis',(-0.851485939575788,0.524377435350472,0.));
#22346=DIRECTION('center_axis',(0.,0.,1.));
#22347=DIRECTION('ref_axis',(0.851485939575788,-0.524377435350471,0.));
#22348=DIRECTION('center_axis',(0.,0.,1.));
#22349=DIRECTION('ref_axis',(0.851485939575788,-0.524377435350471,0.));
#22350=DIRECTION('center_axis',(0.,0.,1.));
#22351=DIRECTION('ref_axis',(0.851485939575788,-0.524377435350471,0.));
#22352=DIRECTION('',(0.671291577386942,-0.413406891836534,-0.615192945271162));
#22353=DIRECTION('center_axis',(0.,0.,1.));
#22354=DIRECTION('ref_axis',(0.851485939575788,-0.524377435350471,0.));
#22355=DIRECTION('center_axis',(0.,0.,1.));
#22356=DIRECTION('ref_axis',(0.851485939575788,-0.524377435350471,0.));
#22357=DIRECTION('center_axis',(0.,0.,1.));
#22358=DIRECTION('ref_axis',(0.851485939575788,-0.524377435350471,0.));
#22359=DIRECTION('center_axis',(0.,0.,1.));
#22360=DIRECTION('ref_axis',(0.851485939575788,-0.524377435350471,0.));
#22361=DIRECTION('center_axis',(0.,0.,1.));
#22362=DIRECTION('ref_axis',(0.851485939575788,-0.524377435350471,0.));
#22363=DIRECTION('center_axis',(0.,0.,1.));
#22364=DIRECTION('ref_axis',(0.851485939575788,-0.524377435350471,0.));
#22365=DIRECTION('center_axis',(0.,0.,1.));
#22366=DIRECTION('ref_axis',(0.851485939575788,-0.524377435350471,0.));
#22367=DIRECTION('center_axis',(0.,0.,1.));
#22368=DIRECTION('ref_axis',(0.851485939575788,-0.524377435350472,0.));
#22369=DIRECTION('center_axis',(0.,0.,1.));
#22370=DIRECTION('ref_axis',(0.851485939575788,-0.524377435350472,0.));
#22371=DIRECTION('center_axis',(0.,0.,1.));
#22372=DIRECTION('ref_axis',(0.851485939575788,-0.524377435350472,0.));
#22373=DIRECTION('',(0.204670796093705,0.841492641219382,-0.499999999999997));
#22374=DIRECTION('',(-0.204670796093705,-0.841492641219382,0.499999999999997));
#22375=DIRECTION('',(0.204670796093705,0.841492641219379,0.500000000000002));
#22376=DIRECTION('',(-0.204670796093705,-0.841492641219379,-0.500000000000002));
#22377=DIRECTION('center_axis',(-0.971672005858197,0.236333478439911,0.));
#22378=DIRECTION('ref_axis',(7.09000435319733E-16,2.91501601757459E-15,
-1.));
#22379=DIRECTION('',(7.09000435319733E-16,2.91501601757459E-15,-1.));
#22380=DIRECTION('center_axis',(7.09000435319733E-16,2.91501601757459E-15,
-1.));
#22381=DIRECTION('ref_axis',(-0.971672005858197,0.236333478439911,-1.18897715061811E-32));
#22382=DIRECTION('center_axis',(-7.09000435319733E-16,-2.91501601757459E-15,
1.));
#22383=DIRECTION('ref_axis',(0.23633347843991,0.971672005858197,3.E-15));
#22384=DIRECTION('center_axis',(7.09000435319733E-16,2.91501601757459E-15,
-1.));
#22385=DIRECTION('ref_axis',(0.236333478439911,0.971672005858197,3.E-15));
#22386=DIRECTION('center_axis',(0.,0.,-1.));
#22387=DIRECTION('ref_axis',(1.,0.,0.));
#22388=DIRECTION('',(7.09000435319733E-16,2.91501601757459E-15,-1.));
#22389=DIRECTION('center_axis',(7.09000435319733E-16,2.91501601757459E-15,
-1.));
#22390=DIRECTION('ref_axis',(0.236333478439911,0.971672005858197,3.E-15));
#22391=DIRECTION('center_axis',(-7.09000435319733E-16,-2.91501601757459E-15,
1.));
#22392=DIRECTION('ref_axis',(-0.153499123700145,0.988148783849521,2.7716385871436E-15));
#22393=DIRECTION('',(7.09000435319733E-16,2.91501601757459E-15,-1.));
#22394=DIRECTION('center_axis',(7.09000435319733E-16,2.91501601757459E-15,
-1.));
#22395=DIRECTION('ref_axis',(0.236333478439911,0.971672005858197,3.E-15));
#22396=DIRECTION('center_axis',(0.,0.,-1.));
#22397=DIRECTION('ref_axis',(-0.236333478439914,-0.971672005858196,0.));
#22398=DIRECTION('center_axis',(0.971672005858197,-0.236333478439911,0.));
#22399=DIRECTION('ref_axis',(-0.236333478439911,-0.971672005858197,-3.E-15));
#22400=DIRECTION('center_axis',(7.09000435319733E-16,2.91501601757459E-15,
-1.));
#22401=DIRECTION('ref_axis',(0.236333478439912,0.971672005858197,4.30631961066728E-15));
#22402=DIRECTION('center_axis',(-0.971672005858197,0.236333478439911,2.95822839457879E-31));
#22403=DIRECTION('ref_axis',(-0.236333478439911,-0.971672005858197,-5.38289951333409E-15));
#22404=DIRECTION('center_axis',(7.09000435319733E-16,2.91501601757459E-15,
-1.));
#22405=DIRECTION('ref_axis',(0.236333478439911,0.971672005858197,2.8421709430404E-15));
#22406=DIRECTION('center_axis',(7.09000435319733E-16,2.91501601757459E-15,
-1.));
#22407=DIRECTION('ref_axis',(0.236333478439912,0.971672005858197,3.E-15));
#22408=DIRECTION('center_axis',(-0.971672005858197,0.236333478439911,-4.93038065763132E-31));
#22409=DIRECTION('ref_axis',(-0.236333478439911,-0.971672005858197,-3.5527136788005E-15));
#22410=DIRECTION('center_axis',(-7.09000435319733E-16,-2.91501601757459E-15,
1.));
#22411=DIRECTION('ref_axis',(0.236333478439911,0.971672005858197,3.E-15));
#22412=DIRECTION('center_axis',(-7.09000435319733E-16,-2.91501601757459E-15,
1.));
#22413=DIRECTION('ref_axis',(0.236333478439911,0.971672005858197,3.E-15));
#22414=DIRECTION('center_axis',(7.09000435319733E-16,2.91501601757459E-15,
-1.));
#22415=DIRECTION('ref_axis',(0.236333478439911,0.971672005858197,3.E-15));
#22416=DIRECTION('center_axis',(-7.09000435319733E-16,-2.91501601757459E-15,
1.));
#22417=DIRECTION('ref_axis',(-0.236333478439911,-0.971672005858197,-3.E-15));
#22418=DIRECTION('',(7.09000435319733E-16,2.91501601757459E-15,-1.));
#22419=DIRECTION('center_axis',(-7.09000435319733E-16,-2.91501601757459E-15,
1.));
#22420=DIRECTION('ref_axis',(-0.236333478439911,-0.971672005858197,-3.E-15));
#22421=DIRECTION('center_axis',(7.09000435319733E-16,2.91501601757459E-15,
-1.));
#22422=DIRECTION('ref_axis',(0.236333478439912,0.971672005858197,3.E-15));
#22423=DIRECTION('center_axis',(-7.09000435319733E-16,-2.91501601757459E-15,
1.));
#22424=DIRECTION('ref_axis',(-0.236333478439912,-0.971672005858197,-3.E-15));
#22425=DIRECTION('',(-7.09000435319733E-16,-2.91501601757459E-15,1.));
#22426=DIRECTION('center_axis',(-7.09000435319733E-16,-2.91501601757459E-15,
1.));
#22427=DIRECTION('ref_axis',(-0.236333478439912,-0.971672005858197,-3.E-15));
#22428=DIRECTION('center_axis',(-7.09000435319733E-16,-2.91501601757459E-15,
1.));
#22429=DIRECTION('ref_axis',(-0.236333478439911,-0.971672005858197,-3.E-15));
#22430=DIRECTION('center_axis',(-7.09000435319733E-16,-2.91501601757459E-15,
1.));
#22431=DIRECTION('ref_axis',(-0.236333478439911,-0.971672005858197,-3.E-15));
#22432=DIRECTION('center_axis',(-7.09000435319733E-16,-2.91501601757459E-15,
1.));
#22433=DIRECTION('ref_axis',(-0.236333478439911,-0.971672005858197,-3.E-15));
#22434=DIRECTION('center_axis',(-7.09000435319733E-16,-2.91501601757459E-15,
1.));
#22435=DIRECTION('ref_axis',(-0.236333478439911,-0.971672005858197,-3.E-15));
#22436=DIRECTION('center_axis',(7.09000435319733E-16,2.91501601757459E-15,
-1.));
#22437=DIRECTION('ref_axis',(0.236333478439911,0.971672005858197,3.E-15));
#22438=DIRECTION('center_axis',(7.09000435319733E-16,2.91501601757459E-15,
-1.));
#22439=DIRECTION('ref_axis',(0.236333478439911,0.971672005858197,3.E-15));
#22440=DIRECTION('center_axis',(7.09000435319733E-16,2.91501601757459E-15,
-1.));
#22441=DIRECTION('ref_axis',(0.236333478439911,0.971672005858197,3.E-15));
#22442=DIRECTION('center_axis',(7.09000435319733E-16,2.91501601757459E-15,
-1.));
#22443=DIRECTION('ref_axis',(0.236333478439911,0.971672005858197,3.E-15));
#22444=DIRECTION('center_axis',(7.09000435319733E-16,2.91501601757459E-15,
-1.));
#22445=DIRECTION('ref_axis',(0.236333478439911,0.971672005858197,3.E-15));
#22446=DIRECTION('',(7.09000435319733E-16,2.91501601757459E-15,-1.));
#22447=DIRECTION('center_axis',(7.09000435319733E-16,2.91501601757459E-15,
-1.));
#22448=DIRECTION('ref_axis',(0.236333478439911,0.971672005858197,3.E-15));
#22449=DIRECTION('center_axis',(7.09000435319733E-16,2.91501601757459E-15,
-1.));
#22450=DIRECTION('ref_axis',(0.236333478439911,0.971672005858197,3.E-15));
#22451=DIRECTION('center_axis',(7.09000435319733E-16,2.91501601757459E-15,
-1.));
#22452=DIRECTION('ref_axis',(0.236333478439911,0.971672005858197,3.E-15));
#22453=DIRECTION('center_axis',(7.09000435319733E-16,2.91501601757459E-15,
-1.));
#22454=DIRECTION('ref_axis',(0.236333478439911,0.971672005858197,3.E-15));
#22455=DIRECTION('center_axis',(7.09000435319733E-16,2.91501601757459E-15,
-1.));
#22456=DIRECTION('ref_axis',(-0.971672005858197,0.236333478439911,-1.18897715061811E-32));
#22457=DIRECTION('center_axis',(7.09000435319733E-16,2.91501601757459E-15,
-1.));
#22458=DIRECTION('ref_axis',(0.236333478439911,0.971672005858197,3.E-15));
#22459=DIRECTION('center_axis',(7.09000435319733E-16,2.91501601757459E-15,
-1.));
#22460=DIRECTION('ref_axis',(-0.971672005858197,0.236333478439911,-1.18897715061811E-32));
#22461=DIRECTION('center_axis',(-7.09000435319733E-16,-2.91501601757459E-15,
1.));
#22462=DIRECTION('ref_axis',(-0.236333478439916,-0.971672005858196,-3.E-15));
#22463=DIRECTION('center_axis',(-7.09000435319733E-16,-2.91501601757459E-15,
1.));
#22464=DIRECTION('ref_axis',(-0.236333478439916,-0.971672005858196,-3.E-15));
#22465=DIRECTION('center_axis',(7.09000435319733E-16,2.91501601757459E-15,
-1.));
#22466=DIRECTION('ref_axis',(-0.971672005858197,0.236333478439911,-1.18897715061811E-32));
#22467=DIRECTION('center_axis',(-7.09000435319733E-16,-2.91501601757459E-15,
1.));
#22468=DIRECTION('ref_axis',(-0.236333478439908,-0.971672005858198,-3.E-15));
#22469=DIRECTION('center_axis',(7.09000435319733E-16,2.91501601757459E-15,
-1.));
#22470=DIRECTION('ref_axis',(-0.971672005858197,0.236333478439911,-1.18897715061811E-32));
#22471=DIRECTION('center_axis',(-7.09000435319733E-16,-2.91501601757459E-15,
1.));
#22472=DIRECTION('ref_axis',(-0.236333478439909,-0.971672005858198,-3.E-15));
#22473=DIRECTION('center_axis',(7.09000435319733E-16,2.91501601757459E-15,
-1.));
#22474=DIRECTION('ref_axis',(-0.971672005858197,0.236333478439911,-1.18897715061811E-32));
#22475=DIRECTION('center_axis',(-7.09000435319733E-16,-2.91501601757459E-15,
1.));
#22476=DIRECTION('ref_axis',(-0.236333478439911,-0.971672005858197,-3.E-15));
#22477=DIRECTION('center_axis',(7.09000435319733E-16,2.91501601757459E-15,
-1.));
#22478=DIRECTION('ref_axis',(0.236333478439916,0.971672005858196,3.E-15));
#22479=DIRECTION('center_axis',(-7.09000435319733E-16,-2.91501601757459E-15,
1.));
#22480=DIRECTION('ref_axis',(-0.236333478439916,-0.971672005858196,-3.E-15));
#22481=DIRECTION('',(7.09000435319733E-16,2.91501601757459E-15,-1.));
#22482=DIRECTION('center_axis',(-7.09000435319733E-16,-2.91501601757459E-15,
1.));
#22483=DIRECTION('ref_axis',(-0.236333478439916,-0.971672005858196,-3.E-15));
#22484=DIRECTION('center_axis',(7.09000435319733E-16,2.91501601757459E-15,
-1.));
#22485=DIRECTION('ref_axis',(0.236333478439908,0.971672005858198,3.E-15));
#22486=DIRECTION('center_axis',(-7.09000435319733E-16,-2.91501601757459E-15,
1.));
#22487=DIRECTION('ref_axis',(-0.236333478439908,-0.971672005858198,-3.E-15));
#22488=DIRECTION('',(7.09000435319733E-16,2.91501601757459E-15,-1.));
#22489=DIRECTION('center_axis',(-7.09000435319733E-16,-2.91501601757459E-15,
1.));
#22490=DIRECTION('ref_axis',(-0.236333478439908,-0.971672005858198,-3.E-15));
#22491=DIRECTION('center_axis',(-7.09000435319733E-16,-2.91501601757459E-15,
1.));
#22492=DIRECTION('ref_axis',(-0.236333478439908,-0.971672005858198,-3.E-15));
#22493=DIRECTION('center_axis',(7.09000435319733E-16,2.91501601757459E-15,
-1.));
#22494=DIRECTION('ref_axis',(0.236333478439909,0.971672005858198,3.E-15));
#22495=DIRECTION('center_axis',(-7.09000435319733E-16,-2.91501601757459E-15,
1.));
#22496=DIRECTION('ref_axis',(-0.236333478439909,-0.971672005858198,-3.E-15));
#22497=DIRECTION('',(7.09000435319733E-16,2.91501601757459E-15,-1.));
#22498=DIRECTION('center_axis',(-7.09000435319733E-16,-2.91501601757459E-15,
1.));
#22499=DIRECTION('ref_axis',(-0.236333478439909,-0.971672005858198,-3.E-15));
#22500=DIRECTION('center_axis',(-7.09000435319733E-16,-2.91501601757459E-15,
1.));
#22501=DIRECTION('ref_axis',(-0.236333478439909,-0.971672005858198,-3.E-15));
#22502=DIRECTION('center_axis',(7.09000435319733E-16,2.91501601757459E-15,
-1.));
#22503=DIRECTION('ref_axis',(0.236333478439911,0.971672005858197,3.E-15));
#22504=DIRECTION('center_axis',(-7.09000435319733E-16,-2.91501601757459E-15,
1.));
#22505=DIRECTION('ref_axis',(-0.236333478439911,-0.971672005858197,-3.E-15));
#22506=DIRECTION('',(7.09000435319733E-16,2.91501601757459E-15,-1.));
#22507=DIRECTION('center_axis',(-7.09000435319733E-16,-2.91501601757459E-15,
1.));
#22508=DIRECTION('ref_axis',(-0.236333478439911,-0.971672005858197,-3.E-15));
#22509=DIRECTION('center_axis',(-7.09000435319733E-16,-2.91501601757459E-15,
1.));
#22510=DIRECTION('ref_axis',(-0.236333478439911,-0.971672005858197,-3.E-15));
#22511=DIRECTION('center_axis',(7.09000435319733E-16,2.91501601757459E-15,
-1.));
#22512=DIRECTION('ref_axis',(0.236333478439911,0.971672005858197,3.E-15));
#22513=DIRECTION('',(7.09000435319733E-16,2.91501601757459E-15,-1.));
#22514=DIRECTION('center_axis',(0.,0.,-1.));
#22515=DIRECTION('ref_axis',(1.,0.,0.));
#22516=DIRECTION('center_axis',(0.236333478439914,0.971672005858196,3.E-15));
#22517=DIRECTION('ref_axis',(-7.09000435319733E-16,-2.91501601757459E-15,
1.));
#22518=DIRECTION('',(0.971672005858196,-0.236333478439914,-9.36576430249746E-30));
#22519=DIRECTION('',(7.09000435319733E-16,2.91501601757459E-15,-1.));
#22520=DIRECTION('',(0.971672005858196,-0.236333478439914,-9.36576430249746E-30));
#22521=DIRECTION('',(7.09000435319733E-16,2.91501601757459E-15,-1.));
#22522=DIRECTION('center_axis',(-0.920977002765036,-0.389616940568464,-1.78871271835535E-15));
#22523=DIRECTION('ref_axis',(7.09000435319733E-16,2.91501601757459E-15,
-1.));
#22524=DIRECTION('',(-0.389616940568464,0.920977002765036,2.40842413440694E-15));
#22525=DIRECTION('',(-0.389616940568464,0.920977002765036,2.40842413440694E-15));
#22526=DIRECTION('',(7.09000435319733E-16,2.91501601757459E-15,-1.));
#22527=DIRECTION('center_axis',(0.36926410344504,0.929324497636284,2.97080420622471E-15));
#22528=DIRECTION('ref_axis',(-7.09000435319733E-16,-2.91501601757459E-15,
1.));
#22529=DIRECTION('',(0.929324497636283,-0.36926410344504,-4.17519302880196E-16));
#22530=DIRECTION('',(0.929324497636283,-0.36926410344504,-4.17519302880196E-16));
#22531=DIRECTION('',(7.09000435319733E-16,2.91501601757459E-15,-1.));
#22532=DIRECTION('center_axis',(-0.966238315689019,-0.257649989898017,-1.43611723392677E-15));
#22533=DIRECTION('ref_axis',(7.09000435319733E-16,2.91501601757459E-15,
-1.));
#22534=DIRECTION('',(-0.257649989898017,0.966238315689019,2.63392621202997E-15));
#22535=DIRECTION('',(-0.257649989898017,0.966238315689019,2.63392621202997E-15));
#22536=DIRECTION('',(7.09000435319733E-16,2.91501601757459E-15,-1.));
#22537=DIRECTION('center_axis',(0.495007422708304,0.868888745158828,2.88378508781496E-15));
#22538=DIRECTION('ref_axis',(-7.09000435319733E-16,-2.91501601757459E-15,
1.));
#22539=DIRECTION('',(0.868888745158828,-0.495007422708304,-8.26912067450997E-16));
#22540=DIRECTION('',(0.868888745158828,-0.495007422708304,-8.26912067450997E-16));
#22541=DIRECTION('',(7.09000435319733E-16,2.91501601757459E-15,-1.));
#22542=DIRECTION('center_axis',(-0.992692898877909,-0.120668175246722,-1.05556936109894E-15));
#22543=DIRECTION('ref_axis',(7.09000435319733E-16,2.91501601757459E-15,
-1.));
#22544=DIRECTION('',(-0.120668175246722,0.992692898877909,2.80816191198249E-15));
#22545=DIRECTION('',(-0.120668175246722,0.992692898877909,2.80816191198249E-15));
#22546=DIRECTION('',(7.09000435319733E-16,2.91501601757459E-15,-1.));
#22547=DIRECTION('center_axis',(0.611115985551149,0.791541061603154,2.7406363729278E-15));
#22548=DIRECTION('ref_axis',(-7.09000435319733E-16,-2.91501601757459E-15,
1.));
#22549=DIRECTION('',(0.791541061603154,-0.611115985551148,-1.2202099292274E-15));
#22550=DIRECTION('',(0.791541061603154,-0.611115985551148,-1.2202099292274E-15));
#22551=DIRECTION('',(7.09000435319733E-16,2.91501601757459E-15,-1.));
#22552=DIRECTION('center_axis',(-0.999825843961577,0.0186623081777341,-6.54476031349669E-16));
#22553=DIRECTION('ref_axis',(7.09000435319733E-16,2.91501601757459E-15,
-1.));
#22554=DIRECTION('',(0.0186623081777341,0.999825843961577,2.92773993455511E-15));
#22555=DIRECTION('',(0.0186623081777341,0.999825843961577,2.92773993455511E-15));
#22556=DIRECTION('',(7.09000435319733E-16,2.91501601757459E-15,-1.));
#22557=DIRECTION('center_axis',(0.71532987086937,0.698786931647988,2.54414428846928E-15));
#22558=DIRECTION('ref_axis',(-7.09000435319733E-16,-2.91501601757459E-15,
1.));
#22559=DIRECTION('',(0.698786931647988,-0.71532987086937,-1.58975779269962E-15));
#22560=DIRECTION('',(0.698786931647988,-0.71532987086937,-1.58975779269962E-15));
#22561=DIRECTION('',(7.09000435319733E-16,2.91501601757459E-15,-1.));
#22562=DIRECTION('center_axis',(-0.987498316277574,0.157629551001571,-2.40644070105632E-16));
#22563=DIRECTION('ref_axis',(7.09000435319733E-16,2.91501601757459E-15,
-1.));
#22564=DIRECTION('',(0.157629551001571,0.987498316277574,2.99033282955644E-15));
#22565=DIRECTION('',(0.157629551001571,0.987498316277574,2.99033282955644E-15));
#22566=DIRECTION('',(7.09000435319733E-16,2.91501601757459E-15,-1.));
#22567=DIRECTION('center_axis',(0.805620673926787,0.592431708926649,2.29813332935694E-15));
#22568=DIRECTION('ref_axis',(-7.09000435319733E-16,-2.91501601757459E-15,
1.));
#22569=DIRECTION('',(0.592431708926649,-0.805620673926787,-1.92836282905961E-15));
#22570=DIRECTION('',(0.592431708926649,-0.805620673926787,-1.92836282905961E-15));
#22571=DIRECTION('',(7.09000435319733E-16,2.91501601757459E-15,-1.));
#22572=DIRECTION('center_axis',(-0.955950257129914,0.293528713916121,1.77871754234442E-16));
#22573=DIRECTION('ref_axis',(0.293528713916121,0.955950257129914,2.99472229748362E-15));
#22574=DIRECTION('',(0.293528713916121,0.955950257129914,2.99472229748362E-15));
#22575=DIRECTION('',(0.293528713916121,0.955950257129914,2.99472229748362E-15));
#22576=DIRECTION('',(7.09000435319733E-16,2.91501601757459E-15,-1.));
#22577=DIRECTION('center_axis',(0.880230986946155,0.474545476872131,2.00739181907658E-15));
#22578=DIRECTION('ref_axis',(-7.09000435319733E-16,-2.91501601757459E-15,
1.));
#22579=DIRECTION('',(0.474545476872131,-0.880230986946155,-2.22943447643218E-15));
#22580=DIRECTION('',(0.474545476872131,-0.880230986946155,-2.22943447643218E-15));
#22581=DIRECTION('',(7.09000435319733E-16,2.91501601757459E-15,-1.));
#22582=DIRECTION('center_axis',(-0.905795713604521,0.423714674298256,5.92925507204465E-16));
#22583=DIRECTION('ref_axis',(0.423714674298256,0.90579571360452,2.94082290233641E-15));
#22584=DIRECTION('',(0.423714674298256,0.905795713604521,2.94082290233641E-15));
#22585=DIRECTION('',(0.423714674298256,0.905795713604521,2.94082290233641E-15));
#22586=DIRECTION('',(7.09000435319733E-16,2.91501601757459E-15,-1.));
#22587=DIRECTION('center_axis',(0.937708605052523,0.347422756897777,1.67757871041224E-15));
#22588=DIRECTION('ref_axis',(-7.09000435319733E-16,-2.91501601757459E-15,
1.));
#22589=DIRECTION('',(0.347422756897777,-0.937708605052523,-2.48711271766512E-15));
#22590=DIRECTION('',(0.347422756897777,-0.937708605052523,-2.48711271766512E-15));
#22591=DIRECTION('',(7.09000435319733E-16,2.91501601757459E-15,-1.));
#22592=DIRECTION('center_axis',(-0.838010886841169,0.545653510513474,9.96438639619516E-16));
#22593=DIRECTION('ref_axis',(0.545653510513474,0.838010886841169,2.82968373453169E-15));
#22594=DIRECTION('',(0.545653510513474,0.838010886841169,2.82968373453169E-15));
#22595=DIRECTION('',(0.545653510513474,0.838010886841169,2.82968373453169E-15));
#22596=DIRECTION('',(7.09000435319733E-16,2.91501601757459E-15,-1.));
#22597=DIRECTION('center_axis',(0.976934791789272,0.213537848147936,1.31511344036723E-15));
#22598=DIRECTION('ref_axis',(-7.09000435319733E-16,-2.91501601757459E-15,
1.));
#22599=DIRECTION('',(0.213537848147936,-0.976934791789272,-2.6963821388975E-15));
#22600=DIRECTION('',(0.213537848147936,-0.976934791789272,-2.6963821388975E-15));
#22601=DIRECTION('',(7.09000435319733E-16,2.91501601757459E-15,-1.));
#22602=DIRECTION('center_axis',(-0.753915131388709,0.656971821818216,1.38055722734653E-15));
#22603=DIRECTION('ref_axis',(0.656971821818216,0.753915131388709,2.66346799155185E-15));
#22604=DIRECTION('',(0.656971821818216,0.753915131388709,2.66346799155185E-15));
#22605=DIRECTION('',(0.656971821818216,0.753915131388709,2.66346799155185E-15));
#22606=DIRECTION('',(7.09000435319733E-16,2.91501601757459E-15,-1.));
#22607=DIRECTION('center_axis',(0.997146054050699,0.0754966680795983,9.27050983124841E-16));
#22608=DIRECTION('ref_axis',(-7.09000435319733E-16,-2.91501601757459E-15,
1.));
#22609=DIRECTION('',(0.0754966680795983,-0.997146054050699,-2.85316954888546E-15));
#22610=DIRECTION('',(0.0754966680795983,-0.997146054050699,-2.85316954888546E-15));
#22611=DIRECTION('',(7.09000435319733E-16,2.91501601757459E-15,-1.));
#22612=DIRECTION('center_axis',(-0.65514527546952,0.755502923905637,1.73780483900381E-15));
#22613=DIRECTION('ref_axis',(0.755502923905637,0.65514527546952,2.4454108737664E-15));
#22614=DIRECTION('',(0.755502923905637,0.65514527546952,2.4454108737664E-15));
#22615=DIRECTION('',(0.755502923905637,0.65514527546952,2.4454108737664E-15));
#22616=DIRECTION('',(7.09000435319733E-16,2.91501601757459E-15,-1.));
#22617=DIRECTION('center_axis',(0.997949002606853,-0.064013968756721,5.20944533000791E-16));
#22618=DIRECTION('ref_axis',(-7.09000435319733E-16,-2.91501601757459E-15,
1.));
#22619=DIRECTION('',(-0.0640139687567209,-0.997949002606853,-2.95442325903662E-15));
#22620=DIRECTION('',(-0.0640139687567209,-0.997949002606853,-2.95442325903662E-15));
#22621=DIRECTION('',(7.09000435319733E-16,2.91501601757459E-15,-1.));
#22622=DIRECTION('center_axis',(-0.543623761980021,0.839329020951075,2.0612280561936E-15));
#22623=DIRECTION('ref_axis',(0.839329020951075,0.543623761980021,2.17975661493672E-15));
#22624=DIRECTION('',(0.839329020951074,0.543623761980021,2.17975661493672E-15));
#22625=DIRECTION('',(0.839329020951074,0.543623761980021,2.17975661493672E-15));
#22626=DIRECTION('',(7.09000435319733E-16,2.91501601757459E-15,-1.));
#22627=DIRECTION('center_axis',(0.979328008977431,-0.202278646506002,1.04698490107502E-16));
#22628=DIRECTION('ref_axis',(-7.09000435319733E-16,-2.91501601757459E-15,
1.));
#22629=DIRECTION('',(-0.202278646506002,-0.979328008977431,-2.99817248105729E-15));
#22630=DIRECTION('',(-0.202278646506002,-0.979328008977431,-2.99817248105729E-15));
#22631=DIRECTION('',(7.09000435319733E-16,2.91501601757459E-15,-1.));
#22632=DIRECTION('center_axis',(-0.421521230326446,0.90681853332631,2.34453181388173E-15));
#22633=DIRECTION('ref_axis',(0.90681853332631,0.421521230326446,1.87167587303369E-15));
#22634=DIRECTION('',(0.90681853332631,0.421521230326446,1.87167587303369E-15));
#22635=DIRECTION('',(0.90681853332631,0.421521230326446,1.87167587303369E-15));
#22636=DIRECTION('',(7.09000435319733E-16,2.91501601757459E-15,-1.));
#22637=DIRECTION('center_axis',(0.941645509622363,-0.336606200489593,-3.13585389802961E-16));
#22638=DIRECTION('ref_axis',(7.09000435319733E-16,2.91501601757459E-15,
-1.));
#22639=DIRECTION('',(-0.336606200489593,-0.941645509622363,-2.98356568610482E-15));
#22640=DIRECTION('',(-0.336606200489593,-0.941645509622363,-2.98356568610482E-15));
#22641=DIRECTION('',(7.09000435319733E-16,2.91501601757459E-15,-1.));
#22642=DIRECTION('center_axis',(-0.29121426739786,0.956657854441141,2.58220192667807E-15));
#22643=DIRECTION('ref_axis',(0.956657854441141,0.29121426739786,1.52716508926182E-15));
#22644=DIRECTION('',(0.956657854441142,0.291214267397859,1.52716508926182E-15));
#22645=DIRECTION('',(0.956657854441142,0.291214267397859,1.52716508926182E-15));
#22646=DIRECTION('',(7.09000435319733E-16,2.91501601757459E-15,-1.));
#22647=DIRECTION('center_axis',(0.885634951528387,-0.464382097664533,-7.25765686799004E-16));
#22648=DIRECTION('ref_axis',(7.09000435319733E-16,2.91501601757459E-15,
-1.));
#22649=DIRECTION('',(-0.464382097664533,-0.885634951528387,-2.91088717882799E-15));
#22650=DIRECTION('',(-0.464382097664533,-0.885634951528387,-2.91088717882799E-15));
#22651=DIRECTION('',(7.09000435319733E-16,2.91501601757459E-15,-1.));
#22652=DIRECTION('center_axis',(-0.155239150005693,0.987876918601457,2.76961241618278E-15));
#22653=DIRECTION('ref_axis',(0.987876918601457,0.155239150005693,1.15292977415201E-15));
#22654=DIRECTION('',(0.987876918601457,0.155239150005693,1.15292977415201E-15));
#22655=DIRECTION('',(0.987876918601457,0.155239150005693,1.15292977415201E-15));
#22656=DIRECTION('',(7.09000435319733E-16,2.91501601757459E-15,-1.));
#22657=DIRECTION('center_axis',(0.812386516497737,-0.583119325535239,-1.12381978024774E-15));
#22658=DIRECTION('ref_axis',(7.09000435319733E-16,2.91501601757459E-15,
-1.));
#22659=DIRECTION('',(-0.583119325535239,-0.812386516497737,-2.78155156370036E-15));
#22660=DIRECTION('',(-0.583119325535239,-0.812386516497737,-2.78155156370036E-15));
#22661=DIRECTION('',(7.09000435319733E-16,2.91501601757459E-15,-1.));
#22662=DIRECTION('center_axis',(-0.0162424791405826,0.999868082234535,2.90311555039392E-15));
#22663=DIRECTION('ref_axis',(0.999868082234536,0.0162424791405826,7.56253992426512E-16));
#22664=DIRECTION('',(0.999868082234535,0.0162424791405826,7.56253992426512E-16));
#22665=DIRECTION('',(0.999868082234535,0.0162424791405826,7.56253992426512E-16));
#22666=DIRECTION('',(7.09000435319733E-16,2.91501601757459E-15,-1.));
#22667=DIRECTION('center_axis',(0.723325901999425,-0.690506799022803,-1.5E-15));
#22668=DIRECTION('ref_axis',(7.09000435319733E-16,2.91501601757459E-15,
-1.));
#22669=DIRECTION('',(-0.690506799022803,-0.723325901999425,-2.59807621135332E-15));
#22670=DIRECTION('',(-0.690506799022803,-0.723325901999425,-2.59807621135332E-15));
#22671=DIRECTION('',(7.09000435319733E-16,2.91501601757459E-15,-1.));
#22672=DIRECTION('center_axis',(0.123070333105456,0.992397950980005,2.98011284266163E-15));
#22673=DIRECTION('ref_axis',(0.992397950980005,-0.123070333105456,3.4485858696459E-16));
#22674=DIRECTION('',(0.992397950980005,-0.123070333105456,3.4485858696459E-16));
#22675=DIRECTION('',(0.992397950980005,-0.123070333105456,3.4485858696459E-16));
#22676=DIRECTION('',(7.09000435319733E-16,2.91501601757459E-15,-1.));
#22677=DIRECTION('center_axis',(0.620186571589713,-0.784454343107231,-1.84698442597697E-15));
#22678=DIRECTION('ref_axis',(7.09000435319733E-16,2.91501601757459E-15,
-1.));
#22679=DIRECTION('',(-0.784454343107231,-0.620186571589714,-2.36403226082017E-15));
#22680=DIRECTION('',(-0.784454343107231,-0.620186571589714,-2.36403226082017E-15));
#22681=DIRECTION('',(7.09000435319733E-16,2.91501601757459E-15,-1.));
#22682=DIRECTION('center_axis',(0.259987721308024,0.965611922445586,2.99910562827505E-15));
#22683=DIRECTION('ref_axis',(-7.09000435319733E-16,-2.91501601757459E-15,
1.));
#22684=DIRECTION('',(0.965611922445586,-0.259987721308024,-7.32490986217644E-17));
#22685=DIRECTION('',(0.965611922445586,-0.259987721308024,-7.32490986217644E-17));
#22686=DIRECTION('',(7.09000435319733E-16,2.91501601757459E-15,-1.));
#22687=DIRECTION('center_axis',(0.504976015015775,-0.863133375706668,-2.15801940101596E-15));
#22688=DIRECTION('ref_axis',(7.09000435319733E-16,2.91501601757459E-15,
-1.));
#22689=DIRECTION('',(-0.863133375706668,-0.504976015015775,-2.08397511137699E-15));
#22690=DIRECTION('',(-0.863133375706668,-0.504976015015775,-2.08397511137699E-15));
#22691=DIRECTION('',(7.09000435319733E-16,2.91501601757459E-15,-1.));
#22692=DIRECTION('center_axis',(0.391844744246979,0.920031356208048,2.95972423426619E-15));
#22693=DIRECTION('ref_axis',(-7.09000435319733E-16,-2.91501601757459E-15,
1.));
#22694=DIRECTION('',(0.920031356208048,-0.391844744246979,-4.89931073823054E-16));
#22695=DIRECTION('',(0.920031356208048,-0.391844744246979,-4.89931073823054E-16));
#22696=DIRECTION('',(7.09000435319733E-16,2.91501601757459E-15,-1.));
#22697=DIRECTION('center_axis',(0.37993667471126,-0.925012498947636,-2.42705098312484E-15));
#22698=DIRECTION('ref_axis',(7.09000435319733E-16,2.91501601757459E-15,
-1.));
#22699=DIRECTION('',(-0.925012498947636,-0.37993667471126,-1.76335575687742E-15));
#22700=DIRECTION('',(-0.925012498947636,-0.37993667471126,-1.76335575687742E-15));
#22701=DIRECTION('',(7.09000435319733E-16,2.91501601757459E-15,-1.));
#22702=DIRECTION('center_axis',(0.516074954955961,0.856543426142074,2.86273517467375E-15));
#22703=DIRECTION('ref_axis',(-7.09000435319733E-16,-2.91501601757459E-15,
1.));
#22704=DIRECTION('',(0.856543426142074,-0.516074954955961,-8.97077097960726E-16));
#22705=DIRECTION('',(0.856543426142074,-0.516074954955961,-8.97077097960726E-16));
#22706=DIRECTION('',(7.09000435319733E-16,2.91501601757459E-15,-1.));
#22707=DIRECTION('center_axis',(0.247502299205053,-0.968887306082711,-2.64884277857678E-15));
#22708=DIRECTION('ref_axis',(7.09000435319733E-16,2.91501601757459E-15,
-1.));
#22709=DIRECTION('',(-0.968887306082711,-0.247502299205053,-1.40841468835767E-15));
#22710=DIRECTION('',(-0.968887306082711,-0.247502299205053,-1.40841468835767E-15));
#22711=DIRECTION('',(7.09000435319733E-16,2.91501601757459E-15,-1.));
#22712=DIRECTION('center_axis',(0.630260353693282,0.776383852589954,2.71002623121929E-15));
#22713=DIRECTION('ref_axis',(-7.09000435319733E-16,-2.91501601757459E-15,
1.));
#22714=DIRECTION('',(0.776383852589954,-0.630260353693282,-1.28676253679666E-15));
#22715=DIRECTION('',(0.776383852589954,-0.630260353693282,-1.28676253679666E-15));
#22716=DIRECTION('',(7.09000435319733E-16,2.91501601757459E-15,-1.));
#22717=DIRECTION('center_axis',(0.110250572974511,-0.993903823897862,-2.81907786235772E-15));
#22718=DIRECTION('ref_axis',(7.09000435319733E-16,2.91501601757459E-15,
-1.));
#22719=DIRECTION('',(-0.993903823897862,-0.110250572974511,-1.02606042997701E-15));
#22720=DIRECTION('',(-0.993903823897862,-0.110250572974511,-1.02606042997701E-15));
#22721=DIRECTION('',(7.09000435319733E-16,2.91501601757459E-15,-1.));
#22722=DIRECTION('center_axis',(0.732178451556494,0.68111285047071,2.50456970978329E-15));
#22723=DIRECTION('ref_axis',(-7.09000435319733E-16,-2.91501601757459E-15,
1.));
#22724=DIRECTION('',(0.68111285047071,-0.732178451556494,-1.65140260652454E-15));
#22725=DIRECTION('',(0.68111285047071,-0.732178451556494,-1.65140260652454E-15));
#22726=DIRECTION('',(7.09000435319733E-16,2.91501601757459E-15,-1.));
#22727=DIRECTION('center_axis',(-0.029147055250812,-0.999575134329684,-2.93444280220142E-15));
#22728=DIRECTION('ref_axis',(7.09000435319733E-16,2.91501601757459E-15,
-1.));
#22729=DIRECTION('',(-0.999575134329684,0.029147055250812,-6.23735072453278E-16));
#22730=DIRECTION('',(-0.999575134329684,0.029147055250812,-6.23735072453278E-16));
#22731=DIRECTION('',(7.09000435319733E-16,2.91501601757459E-15,-1.));
#22732=DIRECTION('center_axis',(0.819845528700799,0.572584761471442,2.25036458785218E-15));
#22733=DIRECTION('ref_axis',(-7.09000435319733E-16,-2.91501601757459E-15,
1.));
#22734=DIRECTION('',(0.572584761471442,-0.819845528700799,-1.98390000295904E-15));
#22735=DIRECTION('',(0.572584761471442,-0.819845528700799,-1.98390000295904E-15));
#22736=DIRECTION('',(7.09000435319733E-16,2.91501601757459E-15,-1.));
#22737=DIRECTION('center_axis',(-0.167977369199961,-0.985790851771642,-2.99269215077947E-15));
#22738=DIRECTION('ref_axis',(7.09000435319733E-16,2.91501601757459E-15,
-1.));
#22739=DIRECTION('',(-0.985790851771642,0.167977369199961,-2.09269421232377E-16));
#22740=DIRECTION('',(-0.985790851771642,0.167977369199961,-2.09269421232377E-16));
#22741=DIRECTION('',(7.09000435319733E-16,2.91501601757459E-15,-1.));
#22742=DIRECTION('center_axis',(0.891555245189413,0.45291196139564,1.9523586789703E-15));
#22743=DIRECTION('ref_axis',(-7.09000435319733E-16,-2.91501601757459E-15,
1.));
#22744=DIRECTION('',(0.45291196139564,-0.891555245189413,-2.27778304248876E-15));
#22745=DIRECTION('',(0.45291196139564,-0.891555245189413,-2.27778304248876E-15));
#22746=DIRECTION('',(7.09000435319733E-16,2.91501601757459E-15,-1.));
#22747=DIRECTION('center_axis',(-0.303538194729059,-0.952819271604339,-2.99269215077947E-15));
#22748=DIRECTION('ref_axis',(7.09000435319733E-16,2.91501601757459E-15,
-1.));
#22749=DIRECTION('',(-0.952819271604339,0.303538194729059,2.09269421232376E-16));
#22750=DIRECTION('',(-0.952819271604339,0.303538194729059,2.09269421232376E-16));
#22751=DIRECTION('',(7.09000435319733E-16,2.91501601757459E-15,-1.));
#22752=DIRECTION('center_axis',(0.945911852959474,0.324423745170996,1.61635232917735E-15));
#22753=DIRECTION('ref_axis',(-7.09000435319733E-16,-2.91501601757459E-15,
1.));
#22754=DIRECTION('',(0.324423745170996,-0.945911852959474,-2.52733162603623E-15));
#22755=DIRECTION('',(0.324423745170996,-0.945911852959474,-2.52733162603623E-15));
#22756=DIRECTION('',(7.09000435319733E-16,2.91501601757459E-15,-1.));
#22757=DIRECTION('center_axis',(-0.433190994567335,-0.901302148131115,-2.93444280220142E-15));
#22758=DIRECTION('ref_axis',(7.09000435319733E-16,2.91501601757459E-15,
-1.));
#22759=DIRECTION('',(-0.901302148131115,0.433190994567335,6.23735072453278E-16));
#22760=DIRECTION('',(-0.901302148131115,0.433190994567335,6.23735072453278E-16));
#22761=DIRECTION('',(7.09000435319733E-16,2.91501601757459E-15,-1.));
#22762=DIRECTION('center_axis',(0.981857362470463,0.18962098977314,1.24888551987049E-15));
#22763=DIRECTION('ref_axis',(-7.09000435319733E-16,-2.91501601757459E-15,
1.));
#22764=DIRECTION('',(0.18962098977314,-0.981857362470463,-2.72768857428003E-15));
#22765=DIRECTION('',(0.18962098977314,-0.981857362470463,-2.72768857428003E-15));
#22766=DIRECTION('',(7.09000435319733E-16,2.91501601757459E-15,-1.));
#22767=DIRECTION('center_axis',(-0.554412224443811,-0.832242203560517,-2.81907786235773E-15));
#22768=DIRECTION('ref_axis',(7.09000435319733E-16,2.91501601757459E-15,
-1.));
#22769=DIRECTION('',(-0.832242203560517,0.554412224443811,1.02606042997701E-15));
#22770=DIRECTION('',(-0.832242203560517,0.554412224443811,1.02606042997701E-15));
#22771=DIRECTION('',(7.09000435319733E-16,2.91501601757459E-15,-1.));
#22772=DIRECTION('center_axis',(0.998692135267162,0.0511274775000253,8.5711057450557E-16));
#22773=DIRECTION('ref_axis',(-7.09000435319733E-16,-2.91501601757459E-15,
1.));
#22774=DIRECTION('',(0.0511274775000253,-0.998692135267162,-2.87495416712523E-15));
#22775=DIRECTION('',(0.0511274775000253,-0.998692135267162,-2.87495416712523E-15));
#22776=DIRECTION('',(7.09000435319733E-16,2.91501601757459E-15,-1.));
#22777=DIRECTION('center_axis',(-0.664842451006046,-0.74698361115909,-2.64884277857678E-15));
#22778=DIRECTION('ref_axis',(7.09000435319733E-16,2.91501601757459E-15,
-1.));
#22779=DIRECTION('',(-0.746983611159089,0.664842451006046,1.40841468835767E-15));
#22780=DIRECTION('',(-0.746983611159089,0.664842451006046,1.40841468835767E-15));
#22781=DIRECTION('',(7.09000435319733E-16,2.91501601757459E-15,-1.));
#22782=DIRECTION('center_axis',(0.996088501646353,-0.0883611729659795,4.48652946756736E-16));
#22783=DIRECTION('ref_axis',(-7.09000435319733E-16,-2.91501601757459E-15,
1.));
#22784=DIRECTION('',(-0.0883611729659795,-0.996088501646353,-2.96626204731923E-15));
#22785=DIRECTION('',(-0.0883611729659795,-0.996088501646353,-2.96626204731923E-15));
#22786=DIRECTION('',(7.09000435319733E-16,2.91501601757459E-15,-1.));
#22787=DIRECTION('center_axis',(-0.762332275506527,-0.647185832447714,-2.42705098312484E-15));
#22788=DIRECTION('ref_axis',(7.09000435319733E-16,2.91501601757459E-15,
-1.));
#22789=DIRECTION('',(-0.647185832447714,0.762332275506527,1.76335575687742E-15));
#22790=DIRECTION('',(-0.647185832447714,0.762332275506527,1.76335575687742E-15));
#22791=DIRECTION('',(7.09000435319733E-16,2.91501601757459E-15,-1.));
#22792=DIRECTION('center_axis',(0.974097138374874,-0.22612997370955,3.14627997344311E-17));
#22793=DIRECTION('ref_axis',(-7.09000435319733E-16,-2.91501601757459E-15,
1.));
#22794=DIRECTION('',(-0.22612997370955,-0.974097138374874,-2.99983501083524E-15));
#22795=DIRECTION('',(-0.22612997370955,-0.974097138374874,-2.99983501083524E-15));
#22796=DIRECTION('',(7.09000435319733E-16,2.91501601757459E-15,-1.));
#22797=DIRECTION('center_axis',(-0.844984169404384,-0.534791317670718,-2.15801940101595E-15));
#22798=DIRECTION('ref_axis',(7.09000435319733E-16,2.91501601757459E-15,
-1.));
#22799=DIRECTION('',(-0.534791317670718,0.844984169404384,2.08397511137699E-15));
#22800=DIRECTION('',(-0.534791317670718,0.844984169404384,2.08397511137699E-15));
#22801=DIRECTION('',(7.09000435319733E-16,2.91501601757459E-15,-1.));
#22802=DIRECTION('center_axis',(0.933146082324,-0.359497411733896,-3.86339734896295E-16));
#22803=DIRECTION('ref_axis',(7.09000435319733E-16,2.91501601757459E-15,
-1.));
#22804=DIRECTION('',(-0.359497411733896,-0.933146082324,-2.97501959812709E-15));
#22805=DIRECTION('',(-0.359497411733896,-0.933146082324,-2.97501959812709E-15));
#22806=DIRECTION('',(7.09000435319733E-16,2.91501601757459E-15,-1.));
#22807=DIRECTION('center_axis',(-0.911189407600033,-0.411987698211368,-1.84698442597698E-15));
#22808=DIRECTION('ref_axis',(7.09000435319733E-16,2.91501601757459E-15,
-1.));
#22809=DIRECTION('',(-0.411987698211368,0.911189407600033,2.36403226082016E-15));
#22810=DIRECTION('',(-0.411987698211368,0.911189407600033,2.36403226082016E-15));
#22811=DIRECTION('',(7.09000435319733E-16,2.91501601757459E-15,-1.));
#22812=DIRECTION('center_axis',(0.874032399218628,-0.485867641561083,-7.96622606042188E-16));
#22813=DIRECTION('ref_axis',(7.09000435319733E-16,2.91501601757459E-15,
-1.));
#22814=DIRECTION('',(-0.485867641561083,-0.874032399218628,-2.89229881297603E-15));
#22815=DIRECTION('',(-0.485867641561083,-0.874032399218628,-2.89229881297603E-15));
#22816=DIRECTION('',(7.09000435319733E-16,2.91501601757459E-15,-1.));
#22817=DIRECTION('center_axis',(-0.959659380439336,-0.281165206835394,-1.5E-15));
#22818=DIRECTION('ref_axis',(7.09000435319733E-16,2.91501601757459E-15,
-1.));
#22819=DIRECTION('',(-0.281165206835394,0.959659380439336,2.59807621135332E-15));
#22820=DIRECTION('',(-0.281165206835394,0.959659380439336,2.59807621135332E-15));
#22821=DIRECTION('',(7.09000435319733E-16,2.91501601757459E-15,-1.));
#22822=DIRECTION('center_axis',(0.797906669659581,-0.60278101041154,-1.19140012430627E-15));
#22823=DIRECTION('ref_axis',(7.09000435319733E-16,2.91501601757459E-15,
-1.));
#22824=DIRECTION('',(-0.60278101041154,-0.797906669659581,-2.75328272137153E-15));
#22825=DIRECTION('',(-0.60278101041154,-0.797906669659581,-2.75328272137153E-15));
#22826=DIRECTION('',(7.09000435319733E-16,2.91501601757459E-15,-1.));
#22827=DIRECTION('center_axis',(-0.989450675034753,-0.144870154529051,-1.12381978024773E-15));
#22828=DIRECTION('ref_axis',(7.09000435319733E-16,2.91501601757459E-15,
-1.));
#22829=DIRECTION('',(-0.144870154529051,0.989450675034753,2.78155156370036E-15));
#22830=DIRECTION('',(-0.144870154529051,0.989450675034753,2.78155156370036E-15));
#22831=DIRECTION('',(7.09000435319733E-16,2.91501601757459E-15,-1.));
#22832=DIRECTION('center_axis',(0.706250594380995,-0.707961932547571,-1.56298839434829E-15));
#22833=DIRECTION('ref_axis',(7.09000435319733E-16,2.91501601757459E-15,
-1.));
#22834=DIRECTION('',(-0.707961932547571,-0.706250594380995,-2.5606771134082E-15));
#22835=DIRECTION('',(-0.707961932547571,-0.706250594380995,-2.5606771134082E-15));
#22836=DIRECTION('',(7.09000435319733E-16,2.91501601757459E-15,-1.));
#22837=DIRECTION('center_axis',(-0.99998343772408,-0.00575536945216082,
-7.25765686799004E-16));
#22838=DIRECTION('ref_axis',(7.09000435319733E-16,2.91501601757459E-15,
-1.));
#22839=DIRECTION('',(-0.00575536945216082,0.99998343772408,2.91088717882799E-15));
#22840=DIRECTION('',(-0.00575536945216082,0.99998343772408,2.91088717882799E-15));
#22841=DIRECTION('',(7.09000435319733E-16,2.91501601757459E-15,-1.));
#22842=DIRECTION('center_axis',(0.600848154630927,-0.799363180961326,-1.90415487316725E-15));
#22843=DIRECTION('ref_axis',(7.09000435319733E-16,2.91501601757459E-15,
-1.));
#22844=DIRECTION('',(-0.799363180961326,-0.600848154630927,-2.31823083815943E-15));
#22845=DIRECTION('',(-0.799363180961326,-0.600848154630927,-2.31823083815943E-15));
#22846=DIRECTION('',(7.09000435319733E-16,2.91501601757459E-15,-1.));
#22847=DIRECTION('center_axis',(-0.991052660262409,0.133471437344482,-3.1358538980296E-16));
#22848=DIRECTION('ref_axis',(7.09000435319733E-16,2.91501601757459E-15,
-1.));
#22849=DIRECTION('',(0.133471437344482,0.991052660262409,2.98356568610482E-15));
#22850=DIRECTION('',(0.133471437344482,0.991052660262409,2.98356568610482E-15));
#22851=DIRECTION('',(7.09000435319733E-16,2.91501601757459E-15,-1.));
#22852=DIRECTION('center_axis',(0.483750889005616,-0.875205734319809,-2.20825914332409E-15));
#22853=DIRECTION('ref_axis',(7.09000435319733E-16,2.91501601757459E-15,
-1.));
#22854=DIRECTION('',(-0.875205734319809,-0.483750889005616,-2.03066283659439E-15));
#22855=DIRECTION('',(-0.875205734319809,-0.483750889005616,-2.03066283659439E-15));
#22856=DIRECTION('',(7.09000435319733E-16,2.91501601757459E-15,-1.));
#22857=DIRECTION('center_axis',(-0.962832170074423,0.270100374434723,1.04698490107504E-16));
#22858=DIRECTION('ref_axis',(0.270100374434723,0.962832170074423,2.99817248105729E-15));
#22859=DIRECTION('',(0.270100374434723,0.962832170074423,2.99817248105729E-15));
#22860=DIRECTION('',(0.270100374434723,0.962832170074423,2.99817248105729E-15));
#22861=DIRECTION('',(7.09000435319733E-16,2.91501601757459E-15,-1.));
#22862=DIRECTION('center_axis',(0.357237962584293,-0.934013403591524,-2.46938216111366E-15));
#22863=DIRECTION('ref_axis',(7.09000435319733E-16,2.91501601757459E-15,
-1.));
#22864=DIRECTION('',(-0.934013403591524,-0.357237962584293,-1.70357029275978E-15));
#22865=DIRECTION('',(-0.934013403591524,-0.357237962584293,-1.70357029275978E-15));
#22866=DIRECTION('',(7.09000435319733E-16,2.91501601757459E-15,-1.));
#22867=DIRECTION('center_axis',(-0.915871246901299,0.401472114971214,5.20944533000789E-16));
#22868=DIRECTION('ref_axis',(0.401472114971214,0.915871246901299,2.95442325903663E-15));
#22869=DIRECTION('',(0.401472114971214,0.915871246901299,2.95442325903662E-15));
#22870=DIRECTION('',(0.401472114971214,0.915871246901299,2.95442325903662E-15));
#22871=DIRECTION('',(7.09000435319733E-16,2.91501601757459E-15,-1.));
#22872=DIRECTION('center_axis',(0.223771805573421,-0.974641564386832,-2.68244146401773E-15));
#22873=DIRECTION('ref_axis',(7.09000435319733E-16,2.91501601757459E-15,
-1.));
#22874=DIRECTION('',(-0.974641564386832,-0.223771805573421,-1.34331969095908E-15));
#22875=DIRECTION('',(-0.974641564386832,-0.223771805573421,-1.34331969095908E-15));
#22876=DIRECTION('',(7.09000435319733E-16,2.91501601757459E-15,-1.));
#22877=DIRECTION('center_axis',(-0.851083931695343,0.525029657457554,9.27050983124842E-16));
#22878=DIRECTION('ref_axis',(0.525029657457554,0.851083931695343,2.85316954888546E-15));
#22879=DIRECTION('',(0.525029657457554,0.851083931695343,2.85316954888546E-15));
#22880=DIRECTION('',(0.525029657457554,0.851083931695343,2.85316954888546E-15));
#22881=DIRECTION('',(7.09000435319733E-16,2.91501601757459E-15,-1.));
#22882=DIRECTION('center_axis',(0.0859501849037209,-0.996299435769697,-2.84329009505664E-15));
#22883=DIRECTION('ref_axis',(7.09000435319733E-16,2.91501601757459E-15,
-1.));
#22884=DIRECTION('',(-0.996299435769697,-0.0859501849037209,-9.56922899377364E-16));
#22885=DIRECTION('',(-0.996299435769697,-0.0859501849037209,-9.56922899377364E-16));
#22886=DIRECTION('',(7.09000435319733E-16,2.91501601757459E-15,-1.));
#22887=DIRECTION('center_axis',(-0.769731235852561,0.638368094873866,1.31511344036723E-15));
#22888=DIRECTION('ref_axis',(0.638368094873866,0.769731235852561,2.6963821388975E-15));
#22889=DIRECTION('',(0.638368094873865,0.769731235852561,2.6963821388975E-15));
#22890=DIRECTION('',(0.638368094873865,0.769731235852561,2.6963821388975E-15));
#22891=DIRECTION('',(7.09000435319733E-16,2.91501601757459E-15,-1.));
#22892=DIRECTION('center_axis',(-0.0535443583482437,-0.998565471909116,
-2.94879731858982E-15));
#22893=DIRECTION('ref_axis',(7.09000435319733E-16,2.91501601757459E-15,
-1.));
#22894=DIRECTION('',(-0.998565471909116,0.0535443583482437,-5.51900692042934E-16));
#22895=DIRECTION('',(-0.998565471909116,0.0535443583482437,-5.51900692042934E-16));
#22896=DIRECTION('',(7.09000435319733E-16,2.91501601757459E-15,-1.));
#22897=DIRECTION('center_axis',(-0.673396597060212,0.739281423456404,1.67757871041224E-15));
#22898=DIRECTION('ref_axis',(0.739281423456404,0.673396597060212,2.48711271766512E-15));
#22899=DIRECTION('',(0.739281423456404,0.673396597060212,2.48711271766512E-15));
#22900=DIRECTION('',(0.739281423456404,0.673396597060212,2.48711271766512E-15));
#22901=DIRECTION('',(7.09000435319733E-16,2.91501601757459E-15,-1.));
#22902=DIRECTION('center_axis',(-0.191996721570762,-0.981395566989213,-2.99690955652389E-15));
#22903=DIRECTION('ref_axis',(7.09000435319733E-16,2.91501601757459E-15,
-1.));
#22904=DIRECTION('',(-0.981395566989213,0.191996721570762,-1.36136365515628E-16));
#22905=DIRECTION('',(-0.981395566989213,0.191996721570762,-1.36136365515628E-16));
#22906=DIRECTION('',(7.09000435319733E-16,2.91501601757459E-15,-1.));
#22907=DIRECTION('center_axis',(-0.563955059483364,0.825805480051516,2.00739181907657E-15));
#22908=DIRECTION('ref_axis',(0.825805480051516,0.563955059483364,2.22943447643218E-15));
#22909=DIRECTION('',(0.825805480051516,0.563955059483364,2.22943447643218E-15));
#22910=DIRECTION('',(0.825805480051516,0.563955059483364,2.22943447643218E-15));
#22911=DIRECTION('',(7.09000435319733E-16,2.91501601757459E-15,-1.));
#22912=DIRECTION('center_axis',(-0.326712087000944,-0.945123913678777,-2.98669035887431E-15));
#22913=DIRECTION('ref_axis',(7.09000435319733E-16,2.91501601757459E-15,
-1.));
#22914=DIRECTION('',(-0.945123913678776,0.326712087000944,2.82277700513634E-16));
#22915=DIRECTION('',(-0.945123913678776,0.326712087000944,2.82277700513634E-16));
#22916=DIRECTION('',(7.09000435319733E-16,2.91501601757459E-15,-1.));
#22917=DIRECTION('center_axis',(-0.443536778163045,0.896256172317238,2.29813332935693E-15));
#22918=DIRECTION('ref_axis',(0.896256172317238,0.443536778163045,1.92836282905962E-15));
#22919=DIRECTION('',(0.896256172317238,0.443536778163045,1.92836282905962E-15));
#22920=DIRECTION('',(0.896256172317238,0.443536778163045,1.92836282905962E-15));
#22921=DIRECTION('',(7.09000435319733E-16,2.91501601757459E-15,-1.));
#22922=DIRECTION('center_axis',(-0.455068373287141,-0.890456498451101,-2.91833863069917E-15));
#22923=DIRECTION('ref_axis',(7.09000435319733E-16,2.91501601757459E-15,
-1.));
#22924=DIRECTION('',(-0.890456498451101,0.455068373287141,6.95197552188514E-16));
#22925=DIRECTION('',(-0.890456498451101,0.455068373287141,6.95197552188514E-16));
#22926=DIRECTION('',(7.09000435319733E-16,2.91501601757459E-15,-1.));
#22927=DIRECTION('center_axis',(-0.314485557971386,0.949262257665091,2.54414428846928E-15));
#22928=DIRECTION('ref_axis',(0.949262257665091,0.314485557971386,1.58975779269962E-15));
#22929=DIRECTION('',(0.949262257665091,0.314485557971386,1.58975779269961E-15));
#22930=DIRECTION('',(0.949262257665091,0.314485557971386,1.58975779269961E-15));
#22931=DIRECTION('',(7.09000435319733E-16,2.91501601757459E-15,-1.));
#22932=DIRECTION('center_axis',(-0.574567271319908,-0.818457360360328,-2.79318476063846E-15));
#22933=DIRECTION('ref_axis',(7.09000435319733E-16,2.91501601757459E-15,
-1.));
#22934=DIRECTION('',(-0.818457360360328,0.574567271319907,1.09458617428554E-15));
#22935=DIRECTION('',(-0.818457360360328,0.574567271319907,1.09458617428554E-15));
#22936=DIRECTION('',(7.09000435319733E-16,2.91501601757459E-15,-1.));
#22937=DIRECTION('center_axis',(-0.179313234115836,0.983792032937307,2.7406363729278E-15));
#22938=DIRECTION('ref_axis',(0.983792032937307,0.179313234115836,1.2202099292274E-15));
#22939=DIRECTION('',(0.983792032937307,0.179313234115836,1.2202099292274E-15));
#22940=DIRECTION('',(0.983792032937307,0.179313234115836,1.2202099292274E-15));
#22941=DIRECTION('',(7.09000435319733E-16,2.91501601757459E-15,-1.));
#22942=DIRECTION('center_axis',(-0.682882870977016,-0.73052788073159,-2.6136647264125E-15));
#22943=DIRECTION('ref_axis',(7.09000435319733E-16,2.91501601757459E-15,
-1.));
#22944=DIRECTION('',(-0.73052788073159,0.682882870977016,1.47266992157342E-15));
#22945=DIRECTION('',(-0.73052788073159,0.682882870977016,1.47266992157342E-15));
#22946=DIRECTION('',(7.09000435319733E-16,2.91501601757459E-15,-1.));
#22947=DIRECTION('center_axis',(-0.0406507821240025,0.99917341533525,2.88378508781496E-15));
#22948=DIRECTION('ref_axis',(0.99917341533525,0.0406507821240025,8.26912067450998E-16));
#22949=DIRECTION('',(0.999173415335249,0.0406507821240025,8.26912067450998E-16));
#22950=DIRECTION('',(0.999173415335249,0.0406507821240025,8.26912067450998E-16));
#22951=DIRECTION('',(7.09000435319733E-16,2.91501601757459E-15,-1.));
#22952=DIRECTION('center_axis',(-0.777906932318306,-0.628379506867564,-2.38327268128649E-15));
#22953=DIRECTION('ref_axis',(7.09000435319733E-16,2.91501601757459E-15,
-1.));
#22954=DIRECTION('',(-0.628379506867564,0.777906932318306,1.82208982397507E-15));
#22955=DIRECTION('',(-0.628379506867564,0.777906932318306,1.82208982397507E-15));
#22956=DIRECTION('',(7.09000435319733E-16,2.91501601757459E-15,-1.));
#22957=DIRECTION('center_axis',(0.0988028911022945,0.995107023746606,2.97080420622471E-15));
#22958=DIRECTION('ref_axis',(0.995107023746606,-0.0988028911022945,4.17519302880201E-16));
#22959=DIRECTION('',(0.995107023746606,-0.0988028911022945,4.17519302880201E-16));
#22960=DIRECTION('',(0.995107023746606,-0.0988028911022945,4.17519302880201E-16));
#22961=DIRECTION('',(7.09000435319733E-16,2.91501601757459E-15,-1.));
#22962=DIRECTION('center_axis',(-0.857789920078043,-0.514000440673454,-2.10649294435173E-15));
#22963=DIRECTION('ref_axis',(7.09000435319733E-16,2.91501601757459E-15,
-1.));
#22964=DIRECTION('',(-0.514000440673454,0.857789920078043,2.13604482054951E-15));
#22965=DIRECTION('',(-0.514000440673454,0.857789920078043,2.13604482054951E-15));
#22966=DIRECTION('center_axis',(-7.09000435319733E-16,-2.91501601757459E-15,
1.));
#22967=DIRECTION('ref_axis',(-0.236333478439911,-0.971672005858197,-3.E-15));
#22968=DIRECTION('center_axis',(-7.09000435319733E-16,-2.91501601757459E-15,
1.));
#22969=DIRECTION('ref_axis',(-0.236333478439911,-0.971672005858197,-3.E-15));
#22970=DIRECTION('center_axis',(-7.09000435319733E-16,-2.91501601757459E-15,
1.));
#22971=DIRECTION('ref_axis',(-0.236333478439911,-0.971672005858197,-3.E-15));
#22972=DIRECTION('center_axis',(0.,0.,1.));
#22973=DIRECTION('ref_axis',(1.,0.,0.));
#22974=DIRECTION('center_axis',(0.,0.,1.));
#22975=DIRECTION('ref_axis',(1.,0.,0.));
#22976=DIRECTION('center_axis',(0.,0.,1.));
#22977=DIRECTION('ref_axis',(1.,0.,0.));
#22978=DIRECTION('center_axis',(0.,0.,1.));
#22979=DIRECTION('ref_axis',(1.,0.,0.));
#22980=DIRECTION('center_axis',(7.09000435319733E-16,2.91501601757459E-15,
-1.));
#22981=DIRECTION('ref_axis',(0.236333478439911,0.971672005858197,3.E-15));
#22982=DIRECTION('center_axis',(-7.09000435319733E-16,-2.91501601757459E-15,
1.));
#22983=DIRECTION('ref_axis',(-0.236333478439911,-0.971672005858197,-3.E-15));
#22984=DIRECTION('center_axis',(-7.09000435319733E-16,-2.91501601757459E-15,
1.));
#22985=DIRECTION('ref_axis',(-0.236333478439911,-0.971672005858197,-3.E-15));
#22986=DIRECTION('',(-7.09000435319733E-16,-2.91501601757459E-15,1.));
#22987=DIRECTION('',(0.204670796093705,0.841492641219382,-0.499999999999997));
#22988=DIRECTION('',(-0.204670796093705,-0.841492641219382,0.499999999999997));
#22989=DIRECTION('center_axis',(0.,0.,1.));
#22990=DIRECTION('ref_axis',(-0.236333478439877,-0.971672005858205,0.));
#22991=DIRECTION('',(-0.204670796093705,-0.841492641219379,-0.500000000000002));
#22992=DIRECTION('',(0.204670796093705,0.841492641219379,0.500000000000002));
#22993=DIRECTION('center_axis',(0.971672005858197,-0.236333478439911,0.));
#22994=DIRECTION('ref_axis',(-0.236333478439911,-0.971672005858197,-3.E-15));
#22995=DIRECTION('center_axis',(-0.971672005858197,0.236333478439911,0.));
#22996=DIRECTION('ref_axis',(7.09000435319733E-16,2.91501601757459E-15,
-1.));
#22997=DIRECTION('',(-7.09000435319733E-16,-2.91501601757459E-15,1.));
#22998=DIRECTION('center_axis',(-9.36335395655066E-14,2.27738783980021E-14,
1.));
#22999=DIRECTION('ref_axis',(-0.236333478439913,-0.971672005858196,0.));
#23000=DIRECTION('center_axis',(-7.09000435319733E-16,-2.91501601757459E-15,
1.));
#23001=DIRECTION('ref_axis',(-0.236333478439908,-0.971672005858198,-3.E-15));
#23002=DIRECTION('center_axis',(-9.36335395655066E-14,2.27738783980021E-14,
1.));
#23003=DIRECTION('ref_axis',(0.999921424989944,-0.0125357028554228,9.39116688816566E-14));
#23004=DIRECTION('center_axis',(7.09000435319733E-16,2.91501601757459E-15,
-1.));
#23005=DIRECTION('ref_axis',(-0.236333478439908,-0.971672005858198,-3.E-15));
#23006=DIRECTION('center_axis',(-7.09000435319733E-16,-2.91501601757459E-15,
1.));
#23007=DIRECTION('ref_axis',(-0.236333478439908,-0.971672005858198,-3.E-15));
#23008=DIRECTION('',(0.167113005226264,0.687075864431466,0.707106781186548));
#23009=DIRECTION('center_axis',(7.09000435319733E-16,2.91501601757459E-15,
-1.));
#23010=DIRECTION('ref_axis',(-0.236333478439911,-0.971672005858197,-3.E-15));
#23011=DIRECTION('center_axis',(7.09000435319733E-16,2.91501601757459E-15,
-1.));
#23012=DIRECTION('ref_axis',(0.236333478439911,0.971672005858197,3.E-15));
#23013=DIRECTION('',(-0.167113005226266,-0.687075864431464,-0.707106781186549));
#23014=DIRECTION('center_axis',(-7.09000435319733E-16,-2.91501601757459E-15,
1.));
#23015=DIRECTION('ref_axis',(-0.236333478439911,-0.971672005858197,-3.E-15));
#23016=DIRECTION('center_axis',(-7.09000435319733E-16,-2.91501601757459E-15,
1.));
#23017=DIRECTION('ref_axis',(-0.236333478439911,-0.971672005858197,-3.E-15));
#23018=DIRECTION('',(-0.167113005226266,-0.687075864431467,-0.707106781186547));
#23019=DIRECTION('center_axis',(7.09000435319733E-16,2.91501601757459E-15,
-1.));
#23020=DIRECTION('ref_axis',(-0.23633347843991,-0.971672005858197,-3.E-15));
#23021=DIRECTION('center_axis',(7.09000435319733E-16,2.91501601757459E-15,
-1.));
#23022=DIRECTION('ref_axis',(0.23633347843991,0.971672005858197,3.E-15));
#23023=DIRECTION('center_axis',(7.09000435319733E-16,2.91501601757459E-15,
-1.));
#23024=DIRECTION('ref_axis',(-0.236333478439911,-0.971672005858197,-3.E-15));
#23025=DIRECTION('',(0.167113005226265,0.687075864431463,0.70710678118655));
#23026=DIRECTION('center_axis',(-7.09000435319733E-16,-2.91501601757459E-15,
1.));
#23027=DIRECTION('ref_axis',(-0.23633347843991,-0.971672005858197,-3.E-15));
#23028=DIRECTION('center_axis',(7.09000435319733E-16,2.91501601757459E-15,
-1.));
#23029=DIRECTION('ref_axis',(0.236333478439911,0.971672005858197,3.E-15));
#23030=DIRECTION('',(-7.09000435319733E-16,-2.91501601757459E-15,1.));
#23031=DIRECTION('center_axis',(-7.09000435319733E-16,-2.91501601757459E-15,
1.));
#23032=DIRECTION('ref_axis',(-0.236333478439911,-0.971672005858197,-3.E-15));
#23033=DIRECTION('center_axis',(-7.09000435319733E-16,-2.91501601757459E-15,
1.));
#23034=DIRECTION('ref_axis',(-0.236333478439911,-0.971672005858197,-3.E-15));
#23035=DIRECTION('center_axis',(7.09000435319733E-16,2.91501601757459E-15,
-1.));
#23036=DIRECTION('ref_axis',(0.236333478439908,0.971672005858198,3.E-15));
#23037=DIRECTION('axis',(0.,0.,1.));
#23038=DIRECTION('refdir',(1.,0.,0.));
#23039=DIRECTION('center_axis',(0.678851252797501,0.734275817779166,-4.75195876958251E-15));
#23040=DIRECTION('ref_axis',(0.734275817779166,-0.678851252797501,1.00517519845672E-30));
#23041=DIRECTION('center_axis',(0.,1.,4.75809867696506E-15));
#23042=DIRECTION('ref_axis',(1.,-3.06753290551076E-28,6.44697202342886E-14));
#23043=DIRECTION('',(0.678851252797501,0.734275817779166,-4.75195876958251E-15));
#23044=DIRECTION('center_axis',(0.678851252797501,0.734275817779166,-4.75195876958251E-15));
#23045=DIRECTION('ref_axis',(0.734275817779166,-0.678851252797501,1.00517519845672E-30));
#23046=DIRECTION('center_axis',(0.678851252797501,0.734275817779166,-4.75195876958251E-15));
#23047=DIRECTION('ref_axis',(-7.E-15,-1.94922383908984E-32,-1.));
#23048=DIRECTION('',(-7.E-15,0.,-1.));
#23049=DIRECTION('center_axis',(0.678851252797502,0.734275817779166,-4.75195876958251E-15));
#23050=DIRECTION('ref_axis',(0.734275817779166,-0.678851252797502,-4.32833613893531E-30));
#23051=DIRECTION('center_axis',(0.678851252797502,0.734275817779166,-4.75195876958251E-15));
#23052=DIRECTION('ref_axis',(0.734275817779166,-0.678851252797502,-4.32833613893531E-30));
#23053=DIRECTION('center_axis',(0.678851252797502,0.734275817779166,-4.75195876958251E-15));
#23054=DIRECTION('ref_axis',(0.734275817779166,-0.678851252797502,-4.32833613893531E-30));
#23055=DIRECTION('center_axis',(-2.31577568721337E-14,1.,3.10052035742355E-14));
#23056=DIRECTION('ref_axis',(1.,2.31577568721319E-14,6.0898447202096E-14));
#23057=DIRECTION('',(0.678851252797502,0.734275817779166,-4.75195876958251E-15));
#23058=DIRECTION('center_axis',(0.678851252797502,0.734275817779166,-4.75195876958251E-15));
#23059=DIRECTION('ref_axis',(0.734275817779166,-0.678851252797502,-4.32833613893531E-30));
#23060=DIRECTION('center_axis',(-9.66488793758498E-15,-1.,6.76542155630949E-29));
#23061=DIRECTION('ref_axis',(7.E-15,6.6510029763507E-46,1.));
#23062=DIRECTION('',(0.867930013859714,-8.38844632162069E-15,0.496686511837674));
#23063=DIRECTION('',(-7.E-15,0.,-1.));
#23064=DIRECTION('',(1.,-9.94102759294464E-15,-7.E-15));
#23065=DIRECTION('',(-7.E-15,0.,-1.));
#23066=DIRECTION('',(-1.,9.91270557701032E-15,7.E-15));
#23067=DIRECTION('',(7.E-15,0.,1.));
#23068=DIRECTION('center_axis',(1.,-9.98518434391482E-15,-7.E-15));
#23069=DIRECTION('ref_axis',(9.98518434391482E-15,1.,-6.98962904074038E-29));
#23070=DIRECTION('',(-7.E-15,0.,-1.));
#23071=DIRECTION('',(9.98518434391482E-15,1.,-6.98962904074038E-29));
#23072=DIRECTION('',(9.98518434391482E-15,1.,-6.98962904074038E-29));
#23073=DIRECTION('center_axis',(7.E-15,0.,1.));
#23074=DIRECTION('ref_axis',(0.,-1.,0.));
#23075=DIRECTION('',(1.,-9.94102759294464E-15,-7.E-15));
#23076=DIRECTION('',(9.98518434391482E-15,1.,-6.98962904074038E-29));
#23077=DIRECTION('center_axis',(1.,-9.98518434391482E-15,-7.E-15));
#23078=DIRECTION('ref_axis',(9.98518434391482E-15,1.,-6.98962904074038E-29));
#23079=DIRECTION('',(-7.E-15,0.,-1.));
#23080=DIRECTION('',(9.98518434391482E-15,1.,-6.98962904074038E-29));
#23081=DIRECTION('center_axis',(-7.E-15,0.,-1.));
#23082=DIRECTION('ref_axis',(-1.,0.,7.E-15));
#23083=DIRECTION('',(-1.,9.91270557701032E-15,7.E-15));
#23084=DIRECTION('',(9.98518434391482E-15,1.,-6.98962904074038E-29));
#23085=DIRECTION('center_axis',(-1.,9.98518434391482E-15,7.E-15));
#23086=DIRECTION('ref_axis',(9.98518434391482E-15,1.,-6.98962904074038E-29));
#23087=DIRECTION('',(7.E-15,0.,1.));
#23088=DIRECTION('',(9.98518434391482E-15,1.,-6.98962904074038E-29));
#23089=DIRECTION('center_axis',(-0.496686511837674,4.95950638183526E-15,
0.867930013859714));
#23090=DIRECTION('ref_axis',(3.98299326130898E-29,-1.,5.71417775931055E-15));
#23091=DIRECTION('',(0.867930013859714,-8.38844632162069E-15,0.496686511837674));
#23092=DIRECTION('center_axis',(4.21032245990148E-13,-1.,-1.056234085578E-14));
#23093=DIRECTION('ref_axis',(1.,4.21032245990149E-13,-7.E-15));
#23094=DIRECTION('',(0.729691385153428,-6.99094164349059E-15,0.683776631973389));
#23095=DIRECTION('',(-7.E-15,0.,-1.));
#23096=DIRECTION('',(-1.,9.66488793758498E-15,7.E-15));
#23097=DIRECTION('',(7.E-15,0.,1.));
#23098=DIRECTION('',(-0.729724964678349,8.12675361862801E-15,-0.683740795861402));
#23099=DIRECTION('',(-7.E-15,0.,-1.));
#23100=DIRECTION('',(9.98518434391482E-15,1.,-6.98962904074038E-29));
#23101=DIRECTION('',(9.98518434391482E-15,1.,-6.98962904074038E-29));
#23102=DIRECTION('',(9.98518434391482E-15,1.,-6.98962904074038E-29));
#23103=DIRECTION('center_axis',(-0.683776631973389,6.82763572031554E-15,
0.729691385153428));
#23104=DIRECTION('ref_axis',(6.59723735469024E-29,-1.,9.35688136002864E-15));
#23105=DIRECTION('',(0.729691385153428,-6.99094164349059E-15,0.683776631973389));
#23106=DIRECTION('',(9.98518434391482E-15,1.,-6.98962904074038E-29));
#23107=DIRECTION('center_axis',(1.,-9.98518434391482E-15,-7.E-15));
#23108=DIRECTION('ref_axis',(9.98518434391482E-15,1.,-6.98962904074038E-29));
#23109=DIRECTION('',(-7.E-15,0.,-1.));
#23110=DIRECTION('',(9.98518434391482E-15,1.,-6.98962904074038E-29));
#23111=DIRECTION('center_axis',(-7.E-15,0.,-1.));
#23112=DIRECTION('ref_axis',(-1.,0.,7.E-15));
#23113=DIRECTION('',(-1.,9.66488793758498E-15,7.E-15));
#23114=DIRECTION('',(9.98518434391482E-15,1.,-6.98962904074038E-29));
#23115=DIRECTION('center_axis',(-1.,9.98518434391482E-15,7.E-15));
#23116=DIRECTION('ref_axis',(9.98518434391482E-15,1.,-6.98962904074038E-29));
#23117=DIRECTION('',(7.E-15,0.,1.));
#23118=DIRECTION('',(9.98518434391482E-15,1.,-6.98962904074038E-29));
#23119=DIRECTION('center_axis',(0.683740795861402,-6.82727789013118E-15,
-0.729724964678349));
#23120=DIRECTION('ref_axis',(9.98518434391482E-15,1.,-6.960711119349E-29));
#23121=DIRECTION('',(-0.729724964678349,8.12675361862801E-15,-0.683740795861402));
#23122=DIRECTION('',(9.98518434391482E-15,1.,-6.98962904074038E-29));
#23123=DIRECTION('',(9.98518434391482E-15,1.,-6.98962904074038E-29));
#23124=DIRECTION('',(9.98518434391482E-15,1.,-6.98962904074038E-29));
#23125=DIRECTION('',(9.98518434391482E-15,1.,-6.98962904074038E-29));
#23126=DIRECTION('center_axis',(1.,-9.98518434391482E-15,-7.E-15));
#23127=DIRECTION('ref_axis',(9.98518434391482E-15,1.,-6.98962904074038E-29));
#23128=DIRECTION('',(-7.E-15,0.,-1.));
#23129=DIRECTION('',(9.98518434391482E-15,1.,-6.98962904074038E-29));
#23130=DIRECTION('center_axis',(7.E-15,0.,1.));
#23131=DIRECTION('ref_axis',(0.,-1.,0.));
#23132=DIRECTION('',(-1.,9.98518434391482E-15,7.E-15));
#23133=DIRECTION('',(-0.734275817779166,0.678851252797501,5.13993072445416E-15));
#23134=DIRECTION('',(-1.,9.98518434391482E-15,7.E-15));
#23135=DIRECTION('',(1.26416333906609E-14,1.,-8.84914337346266E-29));
#23136=DIRECTION('',(-0.774336703951836,-0.632773789685546,5.42035692766285E-15));
#23137=DIRECTION('center_axis',(-9.98518434391482E-15,-1.,6.98962904074038E-29));
#23138=DIRECTION('ref_axis',(7.E-15,1.46992422332527E-45,1.));
#23139=DIRECTION('',(-1.,9.98518434391482E-15,7.E-15));
#23140=DIRECTION('',(7.E-15,0.,1.));
#23141=DIRECTION('',(-7.E-15,0.,-1.));
#23142=DIRECTION('center_axis',(7.E-15,0.,1.));
#23143=DIRECTION('ref_axis',(0.,-1.,0.));
#23144=DIRECTION('',(-1.,9.98518434391482E-15,7.E-15));
#23145=DIRECTION('',(-0.734275817779166,0.678851252797501,5.13993072445416E-15));
#23146=DIRECTION('',(-0.774336703951836,-0.632773789685546,5.42035692766285E-15));
#23147=DIRECTION('center_axis',(-7.E-15,0.,-1.));
#23148=DIRECTION('ref_axis',(-1.,0.,7.E-15));
#23149=DIRECTION('',(-1.,9.98518434391482E-15,7.E-15));
#23150=DIRECTION('',(0.734275817779166,-0.678851252797501,-5.13993072445416E-15));
#23151=DIRECTION('',(-1.,9.98518434391482E-15,7.E-15));
#23152=DIRECTION('',(0.774336703951836,0.632773789685546,-5.42035692766285E-15));
#23153=DIRECTION('center_axis',(-9.98518434391482E-15,-1.,6.98962904074038E-29));
#23154=DIRECTION('ref_axis',(7.E-15,1.46992422332527E-45,1.));
#23155=DIRECTION('',(-1.,9.98518434391482E-15,7.E-15));
#23156=DIRECTION('',(7.E-15,0.,1.));
#23157=DIRECTION('',(-7.E-15,0.,-1.));
#23158=DIRECTION('center_axis',(-7.E-15,0.,-1.));
#23159=DIRECTION('ref_axis',(-1.,0.,7.E-15));
#23160=DIRECTION('',(-1.25743561522893E-14,-1.,8.8020493066025E-29));
#23161=DIRECTION('',(-1.,9.98518434391482E-15,7.E-15));
#23162=DIRECTION('',(0.734275817779166,-0.678851252797501,-5.13993072445416E-15));
#23163=DIRECTION('',(0.774336703951836,0.632773789685546,-5.42035692766285E-15));
#23164=DIRECTION('center_axis',(9.98518434391482E-15,1.,-6.98962904074038E-29));
#23165=DIRECTION('ref_axis',(-1.,9.98518434391482E-15,7.E-15));
#23166=DIRECTION('',(-1.,9.98518434391482E-15,7.E-15));
#23167=DIRECTION('',(-7.E-15,0.,-1.));
#23168=DIRECTION('',(1.,-9.98518434391482E-15,-7.E-15));
#23169=DIRECTION('',(7.E-15,0.,1.));
#23170=DIRECTION('center_axis',(-7.E-15,3.89480588105756E-17,-1.));
#23171=DIRECTION('ref_axis',(-2.7263641167403E-31,-1.,-3.89480588105756E-17));
#23172=DIRECTION('',(-9.97070305550737E-15,-1.,-3.89480588105058E-17));
#23173=DIRECTION('',(-0.734275817779168,0.6788512527975,5.16637066297176E-15));
#23174=DIRECTION('',(-1.,9.98518434391482E-15,7.E-15));
#23175=DIRECTION('',(0.734275817779166,-0.678851252797501,-5.16637066297175E-15));
#23176=DIRECTION('',(0.774336703951836,0.632773789685546,-5.39571161688839E-15));
#23177=DIRECTION('center_axis',(0.678851252797502,0.734275817779166,-4.75195876958251E-15));
#23178=DIRECTION('ref_axis',(-7.E-15,-2.38284042329043E-31,-1.));
#23179=DIRECTION('center_axis',(-0.678851252797498,-0.734275817779169,4.75195876958249E-15));
#23180=DIRECTION('ref_axis',(-0.734275817779169,0.678851252797498,5.15362541093228E-30));
#23181=DIRECTION('center_axis',(0.6788512527975,0.734275817779167,-4.7519587695825E-15));
#23182=DIRECTION('ref_axis',(-7.E-15,5.87886466093466E-32,-1.));
#23183=DIRECTION('center_axis',(-0.678851252797499,-0.734275817779168,4.75195876958249E-15));
#23184=DIRECTION('ref_axis',(-0.734275817779168,0.678851252797499,2.2007191422899E-30));
#23185=DIRECTION('center_axis',(0.678851252797498,0.734275817779169,-4.75195876958249E-15));
#23186=DIRECTION('ref_axis',(0.734275817779169,-0.678851252797498,8.97702189582066E-30));
#23187=DIRECTION('center_axis',(-0.678851252797501,-0.734275817779167,4.75195876958251E-15));
#23188=DIRECTION('ref_axis',(-0.734275817779167,0.678851252797501,-1.38511036298352E-31));
#23189=DIRECTION('',(0.678851252797498,0.734275817779169,-4.75195876958249E-15));
#23190=DIRECTION('center_axis',(0.678851252797499,0.734275817779168,-4.75195876958249E-15));
#23191=DIRECTION('ref_axis',(0.734275817779168,-0.678851252797499,-2.2007191422899E-30));
#23192=DIRECTION('center_axis',(-0.678851252797499,-0.734275817779168,4.75195876958249E-15));
#23193=DIRECTION('ref_axis',(-0.734275817779168,0.678851252797499,2.2007191422899E-30));
#23194=DIRECTION('',(0.678851252797499,0.734275817779168,-4.75195876958249E-15));
#23195=DIRECTION('center_axis',(-6.91154406257336E-15,-8.17791114530617E-17,
-1.));
#23196=DIRECTION('ref_axis',(-1.,-1.87889345193385E-47,6.91154406257336E-15));
#23197=DIRECTION('',(-0.734275817779168,0.6788512527975,5.01946381640023E-15));
#23198=DIRECTION('',(-0.734275817779168,0.6788512527975,5.01946381640023E-15));
#23199=DIRECTION('',(-0.734275817779168,0.6788512527975,5.01946381640023E-15));
#23200=DIRECTION('',(0.6788512527975,0.734275817779168,-4.7519587695825E-15));
#23201=DIRECTION('',(-0.734275817779168,0.6788512527975,5.01946381640023E-15));
#23202=DIRECTION('',(0.6788512527975,0.734275817779168,-4.7519587695825E-15));
#23203=DIRECTION('center_axis',(-0.734275817779168,0.6788512527975,5.13993072445417E-15));
#23204=DIRECTION('ref_axis',(7.E-15,9.60729613809447E-32,1.));
#23205=DIRECTION('',(7.E-15,0.,1.));
#23206=DIRECTION('',(7.E-15,0.,1.));
#23207=DIRECTION('',(0.6788512527975,0.734275817779168,-4.7519587695825E-15));
#23208=DIRECTION('center_axis',(6.90564700007825E-15,8.72310522165992E-17,
1.));
#23209=DIRECTION('ref_axis',(6.10617365516194E-31,-1.,8.72310522165992E-17));
#23210=DIRECTION('',(0.734275817779168,-0.6788512527975,-5.01143268919663E-15));
#23211=DIRECTION('',(0.734275817779168,-0.6788512527975,-5.01143268919663E-15));
#23212=DIRECTION('',(0.734275817779166,-0.678851252797502,-5.01143268919662E-15));
#23213=DIRECTION('',(0.734275817779168,-0.6788512527975,-5.01143268919663E-15));
#23214=DIRECTION('',(0.6788512527975,0.734275817779168,-4.7519587695825E-15));
#23215=DIRECTION('center_axis',(0.734275817779168,-0.6788512527975,-5.13993072445417E-15));
#23216=DIRECTION('ref_axis',(0.6788512527975,0.734275817779168,-4.7519587695825E-15));
#23217=DIRECTION('',(-7.E-15,0.,-1.));
#23218=DIRECTION('',(-7.E-15,0.,-1.));
#23219=DIRECTION('center_axis',(0.6788512527975,0.734275817779168,-4.7519587695825E-15));
#23220=DIRECTION('ref_axis',(-7.E-15,1.36491689365732E-31,-1.));
#23221=DIRECTION('center_axis',(0.6788512527975,0.734275817779168,-4.7519587695825E-15));
#23222=DIRECTION('ref_axis',(-7.E-15,1.36491689365732E-31,-1.));
#23223=DIRECTION('',(-7.E-15,0.,-1.));
#23224=DIRECTION('',(7.E-15,0.,1.));
#23225=DIRECTION('center_axis',(-7.E-15,0.,-1.));
#23226=DIRECTION('ref_axis',(-1.,0.,7.E-15));
#23227=DIRECTION('',(1.,-2.32761274233658E-16,-7.E-15));
#23228=DIRECTION('',(-0.734275817779166,0.678851252797502,5.13993072445416E-15));
#23229=DIRECTION('',(-1.,0.,7.E-15));
#23230=DIRECTION('',(0.734275817779166,-0.678851252797501,-5.13993072445416E-15));
#23231=DIRECTION('center_axis',(-7.E-15,0.,-1.));
#23232=DIRECTION('ref_axis',(-1.,0.,7.E-15));
#23233=DIRECTION('center_axis',(-7.E-15,0.,-1.));
#23234=DIRECTION('ref_axis',(-1.,0.,7.E-15));
#23235=DIRECTION('center_axis',(-7.E-15,0.,-1.));
#23236=DIRECTION('ref_axis',(-1.,0.,7.E-15));
#23237=DIRECTION('',(1.,-2.32761274233658E-16,-7.E-15));
#23238=DIRECTION('',(0.734275817779166,-0.678851252797501,-5.13993072445416E-15));
#23239=DIRECTION('',(-1.,0.,7.E-15));
#23240=DIRECTION('',(-0.734275817779166,0.678851252797502,5.13993072445416E-15));
#23241=DIRECTION('center_axis',(-7.E-15,0.,-1.));
#23242=DIRECTION('ref_axis',(-1.,0.,7.E-15));
#23243=DIRECTION('center_axis',(-7.E-15,0.,-1.));
#23244=DIRECTION('ref_axis',(-1.,0.,7.E-15));
#23245=DIRECTION('center_axis',(0.678851252797502,0.734275817779166,-4.75195876958251E-15));
#23246=DIRECTION('ref_axis',(-7.E-15,-2.38284042329043E-31,-1.));
#23247=DIRECTION('',(7.E-15,0.,1.));
#23248=DIRECTION('',(7.E-15,0.,1.));
#23249=DIRECTION('',(7.E-15,0.,1.));
#23250=DIRECTION('center_axis',(7.E-15,0.,1.));
#23251=DIRECTION('ref_axis',(1.,0.,-7.E-15));
#23252=DIRECTION('',(7.E-15,0.,1.));
#23253=DIRECTION('center_axis',(7.E-15,0.,1.));
#23254=DIRECTION('ref_axis',(1.,0.,-7.E-15));
#23255=DIRECTION('',(7.E-15,0.,1.));
#23256=DIRECTION('center_axis',(0.,1.,0.));
#23257=DIRECTION('ref_axis',(-1.,0.,7.E-15));
#23258=DIRECTION('',(7.E-15,0.,1.));
#23259=DIRECTION('center_axis',(-0.678851252797501,-0.734275817779166,4.75195876958251E-15));
#23260=DIRECTION('ref_axis',(7.E-15,1.94922383908984E-32,1.));
#23261=DIRECTION('',(-7.E-15,0.,-1.));
#23262=DIRECTION('',(-0.734275817779166,0.678851252797501,5.13993072445416E-15));
#23263=DIRECTION('',(7.E-15,0.,1.));
#23264=DIRECTION('',(7.E-15,0.,1.));
#23265=DIRECTION('',(-0.734275817779168,0.6788512527975,5.13993072445417E-15));
#23266=DIRECTION('center_axis',(-2.32761274233658E-16,-1.,1.6293289196356E-30));
#23267=DIRECTION('ref_axis',(7.E-15,-4.06124814761934E-47,1.));
#23268=DIRECTION('',(7.E-15,0.,1.));
#23269=DIRECTION('center_axis',(-0.678851252797501,-0.734275817779166,4.75195876958251E-15));
#23270=DIRECTION('ref_axis',(7.E-15,1.94922383908984E-32,1.));
#23271=DIRECTION('center_axis',(0.678851252797502,0.734275817779166,-4.75195876958251E-15));
#23272=DIRECTION('ref_axis',(0.734275817779166,-0.678851252797502,3.17141862916252E-30));
#23273=DIRECTION('center_axis',(-0.678851252797501,-0.734275817779166,4.75195876958251E-15));
#23274=DIRECTION('ref_axis',(7.E-15,1.94922383908984E-32,1.));
#23275=DIRECTION('center_axis',(0.678851252797499,0.734275817779168,-4.75195876958249E-15));
#23276=DIRECTION('ref_axis',(0.734275817779168,-0.678851252797499,-5.62097512108036E-30));
#23277=DIRECTION('center_axis',(-0.678851252797499,-0.734275817779168,4.75195876958249E-15));
#23278=DIRECTION('ref_axis',(-0.734275817779168,0.678851252797499,7.56831899889172E-30));
#23279=DIRECTION('center_axis',(0.678851252797499,0.734275817779168,-4.75195876958249E-15));
#23280=DIRECTION('ref_axis',(0.734275817779168,-0.678851252797499,-6.20021660737553E-30));
#23281=DIRECTION('',(-0.678851252797499,-0.734275817779168,4.75195876958249E-15));
#23282=DIRECTION('center_axis',(-0.6788512527975,-0.734275817779167,4.7519587695825E-15));
#23283=DIRECTION('ref_axis',(-0.734275817779167,0.6788512527975,2.81659329962846E-30));
#23284=DIRECTION('center_axis',(0.678851252797499,0.734275817779168,-4.75195876958249E-15));
#23285=DIRECTION('ref_axis',(0.734275817779168,-0.678851252797499,-5.62097512108036E-30));
#23286=DIRECTION('',(-0.6788512527975,-0.734275817779167,4.7519587695825E-15));
#23287=DIRECTION('center_axis',(7.E-15,0.,1.));
#23288=DIRECTION('ref_axis',(0.,-1.,0.));
#23289=DIRECTION('',(-0.734275817779168,0.6788512527975,5.13993072445417E-15));
#23290=DIRECTION('',(-0.734275817779168,0.6788512527975,5.13993072445417E-15));
#23291=DIRECTION('',(-0.6788512527975,-0.734275817779168,4.7519587695825E-15));
#23292=DIRECTION('',(-0.734275817779168,0.6788512527975,5.13993072445417E-15));
#23293=DIRECTION('',(-0.6788512527975,-0.734275817779168,4.7519587695825E-15));
#23294=DIRECTION('center_axis',(-0.734275817779167,0.6788512527975,5.13993072445417E-15));
#23295=DIRECTION('ref_axis',(7.E-15,9.31258724118286E-32,1.));
#23296=DIRECTION('',(-7.E-15,0.,-1.));
#23297=DIRECTION('',(-0.6788512527975,-0.734275817779168,4.7519587695825E-15));
#23298=DIRECTION('center_axis',(-7.E-15,0.,-1.));
#23299=DIRECTION('ref_axis',(-1.,0.,7.E-15));
#23300=DIRECTION('',(0.734275817779168,-0.6788512527975,-5.13993072445418E-15));
#23301=DIRECTION('',(0.734275817779168,-0.6788512527975,-5.13993072445417E-15));
#23302=DIRECTION('',(0.734275817779168,-0.6788512527975,-5.13993072445417E-15));
#23303=DIRECTION('',(-0.6788512527975,-0.734275817779168,4.7519587695825E-15));
#23304=DIRECTION('center_axis',(0.734275817779167,-0.6788512527975,-5.37545456543899E-15));
#23305=DIRECTION('ref_axis',(0.6788512527975,0.734275817779167,-4.7519587695825E-15));
#23306=DIRECTION('',(7.E-15,-3.46944695195362E-16,1.));
#23307=DIRECTION('',(7.E-15,-3.46944695195362E-16,1.));
#23308=DIRECTION('center_axis',(-0.6788512527975,-0.734275817779167,4.49720566979378E-15));
#23309=DIRECTION('ref_axis',(7.E-15,-3.46944695195361E-16,1.));
#23310=DIRECTION('center_axis',(-7.E-15,0.,-1.));
#23311=DIRECTION('ref_axis',(-1.,0.,7.E-15));
#23312=DIRECTION('',(0.774336703951835,0.632773789685546,-5.42035692766285E-15));
#23313=DIRECTION('',(0.734275817779166,-0.678851252797501,-5.13993072445416E-15));
#23314=DIRECTION('',(1.,3.96829847184794E-16,-7.E-15));
#23315=DIRECTION('center_axis',(-7.E-15,0.,-1.));
#23316=DIRECTION('ref_axis',(-1.,0.,7.E-15));
#23317=DIRECTION('',(0.,1.,0.));
#23318=DIRECTION('',(0.774336703951835,0.632773789685546,-5.42035692766285E-15));
#23319=DIRECTION('',(1.,3.96829847184794E-16,-7.E-15));
#23320=DIRECTION('',(0.734275817779166,-0.678851252797501,-5.13993072445416E-15));
#23321=DIRECTION('',(-1.,0.,7.E-15));
#23322=DIRECTION('',(-0.734275817779168,0.6788512527975,5.13993072445417E-15));
#23323=DIRECTION('center_axis',(0.6788512527975,0.734275817779167,-4.7519587695825E-15));
#23324=DIRECTION('ref_axis',(-7.E-15,5.87886466093466E-32,-1.));
#23325=DIRECTION('',(7.E-15,0.,1.));
#23326=DIRECTION('',(7.E-15,0.,1.));
#23327=DIRECTION('',(7.E-15,0.,1.));
#23328=DIRECTION('center_axis',(0.,1.,0.));
#23329=DIRECTION('ref_axis',(-1.,0.,7.E-15));
#23330=DIRECTION('',(7.E-15,0.,1.));
#23331=DIRECTION('',(7.E-15,0.,1.));
#23332=DIRECTION('',(7.E-15,0.,1.));
#23333=DIRECTION('center_axis',(-0.678851252797501,-0.734275817779166,4.75195876958251E-15));
#23334=DIRECTION('ref_axis',(7.E-15,1.94922383908984E-32,1.));
#23335=DIRECTION('',(7.E-15,0.,1.));
#23336=DIRECTION('',(7.E-15,0.,1.));
#23337=DIRECTION('',(7.E-15,0.,1.));
#23338=DIRECTION('center_axis',(3.96829847184794E-16,-1.,-2.77780893029356E-30));
#23339=DIRECTION('ref_axis',(1.,3.96829847184794E-16,-7.E-15));
#23340=DIRECTION('',(7.E-15,0.,1.));
#23341=DIRECTION('center_axis',(0.632773789685546,-0.774336703951836,-4.42941652779882E-15));
#23342=DIRECTION('ref_axis',(0.774336703951836,0.632773789685546,-5.42035692766285E-15));
#23343=DIRECTION('',(7.E-15,0.,1.));
#23344=DIRECTION('center_axis',(1.,0.,-7.E-15));
#23345=DIRECTION('ref_axis',(-7.E-15,0.,-1.));
#23346=DIRECTION('',(7.E-15,0.,1.));
#23347=DIRECTION('',(7.E-15,0.,1.));
#23348=DIRECTION('center_axis',(-0.6788512527975,-0.734275817779167,4.49720566979378E-15));
#23349=DIRECTION('ref_axis',(7.E-15,-3.46944695195361E-16,1.));
#23350=DIRECTION('center_axis',(3.96829847184794E-16,-1.,-2.77780893029356E-30));
#23351=DIRECTION('ref_axis',(1.,3.96829847184794E-16,-7.E-15));
#23352=DIRECTION('',(7.E-15,0.,1.));
#23353=DIRECTION('center_axis',(0.632773789685546,-0.774336703951836,-4.42941652779882E-15));
#23354=DIRECTION('ref_axis',(0.774336703951836,0.632773789685546,-5.42035692766285E-15));
#23355=DIRECTION('center_axis',(-9.98518434391482E-15,-1.,6.98962904074038E-29));
#23356=DIRECTION('ref_axis',(7.E-15,1.46992422332527E-45,1.));
#23357=DIRECTION('axis',(0.,0.,1.));
#23358=DIRECTION('refdir',(1.,0.,0.));
#23359=DIRECTION('center_axis',(0.,0.,1.));
#23360=DIRECTION('ref_axis',(1.,0.,0.));
#23361=DIRECTION('center_axis',(0.,0.,1.));
#23362=DIRECTION('ref_axis',(1.,0.,0.));
#23363=DIRECTION('center_axis',(0.,0.,-1.));
#23364=DIRECTION('ref_axis',(1.,0.,0.));
#23365=DIRECTION('center_axis',(0.,0.,1.));
#23366=DIRECTION('ref_axis',(1.,0.,0.));
#23367=DIRECTION('center_axis',(0.,0.,1.));
#23368=DIRECTION('ref_axis',(1.,0.,0.));
#23369=DIRECTION('center_axis',(0.,0.,1.));
#23370=DIRECTION('ref_axis',(1.,0.,0.));
#23371=DIRECTION('',(0.707106781186548,8.65956056235494E-17,-0.707106781186547));
#23372=DIRECTION('center_axis',(0.,0.,1.));
#23373=DIRECTION('ref_axis',(0.990993942369174,-0.133906707029938,0.));
#23374=DIRECTION('',(0.,0.,1.));
#23375=DIRECTION('center_axis',(0.,0.,-1.));
#23376=DIRECTION('ref_axis',(-1.,0.,0.));
#23377=DIRECTION('',(0.,0.,-1.));
#23378=DIRECTION('',(0.,0.,-1.));
#23379=DIRECTION('center_axis',(0.,0.,-1.));
#23380=DIRECTION('ref_axis',(1.,0.,0.));
#23381=DIRECTION('center_axis',(0.,0.,-1.));
#23382=DIRECTION('ref_axis',(-1.,0.,0.));
#23383=DIRECTION('',(0.,0.,-1.));
#23384=DIRECTION('center_axis',(0.,0.,-1.));
#23385=DIRECTION('ref_axis',(-1.,0.,0.));
#23386=DIRECTION('',(0.,0.,-1.));
#23387=DIRECTION('center_axis',(0.,0.,-1.));
#23388=DIRECTION('ref_axis',(-1.,0.,0.));
#23389=DIRECTION('',(0.,0.,-1.));
#23390=DIRECTION('center_axis',(0.,0.,-1.));
#23391=DIRECTION('ref_axis',(-1.,0.,0.));
#23392=DIRECTION('',(0.,0.,-1.));
#23393=DIRECTION('center_axis',(0.,0.,-1.));
#23394=DIRECTION('ref_axis',(-1.,0.,0.));
#23395=DIRECTION('',(0.,0.,-1.));
#23396=DIRECTION('center_axis',(0.,0.,-1.));
#23397=DIRECTION('ref_axis',(-1.,0.,0.));
#23398=DIRECTION('',(0.,0.,-1.));
#23399=DIRECTION('center_axis',(0.,0.,-1.));
#23400=DIRECTION('ref_axis',(-1.,0.,0.));
#23401=DIRECTION('',(0.,0.,-1.));
#23402=DIRECTION('center_axis',(0.,0.,-1.));
#23403=DIRECTION('ref_axis',(-1.,0.,0.));
#23404=DIRECTION('',(0.,0.,-1.));
#23405=DIRECTION('center_axis',(0.,0.,-1.));
#23406=DIRECTION('ref_axis',(-1.,0.,0.));
#23407=DIRECTION('',(0.,0.,-1.));
#23408=DIRECTION('center_axis',(0.,0.,-1.));
#23409=DIRECTION('ref_axis',(-1.,0.,0.));
#23410=DIRECTION('',(0.,0.,-1.));
#23411=DIRECTION('center_axis',(0.,0.,-1.));
#23412=DIRECTION('ref_axis',(-1.,0.,0.));
#23413=DIRECTION('',(0.,0.,-1.));
#23414=DIRECTION('center_axis',(0.,0.,-1.));
#23415=DIRECTION('ref_axis',(-1.,0.,0.));
#23416=DIRECTION('',(0.,0.,-1.));
#23417=DIRECTION('center_axis',(0.,0.,-1.));
#23418=DIRECTION('ref_axis',(-1.,0.,0.));
#23419=DIRECTION('',(0.,0.,-1.));
#23420=DIRECTION('center_axis',(0.,0.,1.));
#23421=DIRECTION('ref_axis',(1.,0.,0.));
#23422=DIRECTION('center_axis',(0.,0.,1.));
#23423=DIRECTION('ref_axis',(1.,-7.27351010247249E-15,0.));
#23424=DIRECTION('',(0.,0.,-1.));
#23425=DIRECTION('',(0.,0.,1.));
#23426=DIRECTION('center_axis',(0.,0.,1.));
#23427=DIRECTION('ref_axis',(1.,-7.27351010247249E-15,0.));
#23428=DIRECTION('',(0.,0.,-1.));
#23429=DIRECTION('center_axis',(0.,0.,1.));
#23430=DIRECTION('ref_axis',(1.,-7.27351010247249E-15,0.));
#23431=DIRECTION('',(0.,0.,-1.));
#23432=DIRECTION('center_axis',(0.,0.,1.));
#23433=DIRECTION('ref_axis',(1.,-7.27351010247249E-15,0.));
#23434=DIRECTION('',(0.,0.,-1.));
#23435=DIRECTION('center_axis',(0.,0.,1.));
#23436=DIRECTION('ref_axis',(1.,-7.27351010247249E-15,0.));
#23437=DIRECTION('',(0.,0.,-1.));
#23438=DIRECTION('center_axis',(0.,0.,1.));
#23439=DIRECTION('ref_axis',(1.,-7.27351010247249E-15,0.));
#23440=DIRECTION('',(0.,0.,-1.));
#23441=DIRECTION('center_axis',(0.,0.,1.));
#23442=DIRECTION('ref_axis',(1.,-7.27351010247249E-15,0.));
#23443=DIRECTION('',(0.,0.,-1.));
#23444=DIRECTION('center_axis',(0.,0.,1.));
#23445=DIRECTION('ref_axis',(1.,-7.27351010247249E-15,0.));
#23446=DIRECTION('',(0.,0.,-1.));
#23447=DIRECTION('center_axis',(0.,0.,1.));
#23448=DIRECTION('ref_axis',(1.,-7.27351010247249E-15,0.));
#23449=DIRECTION('',(0.,0.,-1.));
#23450=DIRECTION('center_axis',(0.,0.,1.));
#23451=DIRECTION('ref_axis',(1.,-7.27351010247249E-15,0.));
#23452=DIRECTION('',(0.,0.,-1.));
#23453=DIRECTION('center_axis',(0.,0.,1.));
#23454=DIRECTION('ref_axis',(1.,-7.27351010247249E-15,0.));
#23455=DIRECTION('',(0.,0.,-1.));
#23456=DIRECTION('center_axis',(0.,0.,1.));
#23457=DIRECTION('ref_axis',(1.,-7.27351010247249E-15,0.));
#23458=DIRECTION('',(0.,0.,-1.));
#23459=DIRECTION('center_axis',(0.,0.,1.));
#23460=DIRECTION('ref_axis',(1.,-7.27351010247249E-15,0.));
#23461=DIRECTION('',(0.,0.,-1.));
#23462=DIRECTION('center_axis',(0.,0.,1.));
#23463=DIRECTION('ref_axis',(1.,-7.27351010247249E-15,0.));
#23464=DIRECTION('',(0.,0.,-1.));
#23465=DIRECTION('',(0.,0.,-1.));
#23466=DIRECTION('center_axis',(0.,0.,1.));
#23467=DIRECTION('ref_axis',(1.,0.,0.));
#23468=DIRECTION('center_axis',(0.,0.,1.));
#23469=DIRECTION('ref_axis',(1.,0.,0.));
#23470=DIRECTION('',(0.,0.,-1.));
#23471=DIRECTION('center_axis',(0.,0.,1.));
#23472=DIRECTION('ref_axis',(0.999820197862873,-0.0189623823779183,0.));
#23473=DIRECTION('center_axis',(0.,0.,1.));
#23474=DIRECTION('ref_axis',(1.,0.,0.));
#23475=DIRECTION('center_axis',(0.,0.,-1.));
#23476=DIRECTION('ref_axis',(-0.990993942369175,0.133906707029934,0.));
#23477=DIRECTION('',(0.,0.,-1.));
#23478=DIRECTION('center_axis',(0.,0.,1.));
#23479=DIRECTION('ref_axis',(1.,0.,0.));
#23480=DIRECTION('center_axis',(0.,0.,-1.));
#23481=DIRECTION('ref_axis',(-1.,0.,0.));
#23482=DIRECTION('center_axis',(0.,0.,1.));
#23483=DIRECTION('ref_axis',(0.990993942369174,-0.133906707029939,0.));
#23484=DIRECTION('',(0.,0.,1.));
#23485=DIRECTION('center_axis',(0.,0.,-1.));
#23486=DIRECTION('ref_axis',(1.,0.,0.));
#23487=DIRECTION('center_axis',(0.,0.,1.));
#23488=DIRECTION('ref_axis',(1.,0.,0.));
#23489=DIRECTION('center_axis',(0.,0.,1.));
#23490=DIRECTION('ref_axis',(1.,0.,0.));
#23491=DIRECTION('center_axis',(0.,-1.,0.));
#23492=DIRECTION('ref_axis',(-1.,0.,0.));
#23493=DIRECTION('center_axis',(0.,0.,-1.));
#23494=DIRECTION('ref_axis',(1.,0.,0.));
#23495=DIRECTION('center_axis',(0.,0.,-1.));
#23496=DIRECTION('ref_axis',(1.,0.,0.));
#23497=DIRECTION('center_axis',(0.,0.,1.));
#23498=DIRECTION('ref_axis',(1.,0.,0.));
#23499=DIRECTION('center_axis',(0.,0.,1.));
#23500=DIRECTION('ref_axis',(1.,0.,0.));
#23501=DIRECTION('center_axis',(0.,0.,1.));
#23502=DIRECTION('ref_axis',(1.,0.,0.));
#23503=DIRECTION('center_axis',(0.,-1.,0.));
#23504=DIRECTION('ref_axis',(-1.,0.,0.));
#23505=DIRECTION('center_axis',(0.,0.,-1.));
#23506=DIRECTION('ref_axis',(1.,0.,0.));
#23507=DIRECTION('center_axis',(0.,0.,1.));
#23508=DIRECTION('ref_axis',(1.,0.,0.));
#23509=DIRECTION('center_axis',(0.,0.,1.));
#23510=DIRECTION('ref_axis',(1.,0.,0.));
#23511=DIRECTION('center_axis',(0.,0.,1.));
#23512=DIRECTION('ref_axis',(1.,0.,0.));
#23513=DIRECTION('center_axis',(0.,-1.,0.));
#23514=DIRECTION('ref_axis',(-1.,0.,0.));
#23515=DIRECTION('center_axis',(0.,0.,-1.));
#23516=DIRECTION('ref_axis',(1.,0.,0.));
#23517=DIRECTION('center_axis',(0.,0.,1.));
#23518=DIRECTION('ref_axis',(1.,0.,0.));
#23519=DIRECTION('center_axis',(0.,0.,1.));
#23520=DIRECTION('ref_axis',(1.,0.,0.));
#23521=DIRECTION('center_axis',(0.,-1.,0.));
#23522=DIRECTION('ref_axis',(-1.,0.,0.));
#23523=DIRECTION('center_axis',(0.,0.,-1.));
#23524=DIRECTION('ref_axis',(1.,0.,0.));
#23525=DIRECTION('center_axis',(0.,0.,-1.));
#23526=DIRECTION('ref_axis',(1.,0.,0.));
#23527=DIRECTION('center_axis',(0.,0.,-1.));
#23528=DIRECTION('ref_axis',(-1.,0.,0.));
#23529=DIRECTION('',(0.,0.,-1.));
#23530=DIRECTION('center_axis',(0.,0.,-1.));
#23531=DIRECTION('ref_axis',(-1.,0.,0.));
#23532=DIRECTION('',(0.,0.,1.));
#23533=DIRECTION('center_axis',(0.,0.,1.));
#23534=DIRECTION('ref_axis',(1.,0.,0.));
#23535=DIRECTION('center_axis',(0.,0.,1.));
#23536=DIRECTION('ref_axis',(1.,0.,0.));
#23537=DIRECTION('center_axis',(0.,0.,1.));
#23538=DIRECTION('ref_axis',(1.,0.,0.));
#23539=DIRECTION('center_axis',(0.,0.,1.));
#23540=DIRECTION('ref_axis',(1.,0.,0.));
#23541=DIRECTION('center_axis',(0.,0.,1.));
#23542=DIRECTION('ref_axis',(1.,0.,0.));
#23543=DIRECTION('center_axis',(0.,0.,1.));
#23544=DIRECTION('ref_axis',(-0.925614790208249,-0.378466986866409,0.));
#23545=DIRECTION('center_axis',(0.,0.,1.));
#23546=DIRECTION('ref_axis',(1.,0.,0.));
#23547=DIRECTION('center_axis',(0.,0.,1.));
#23548=DIRECTION('ref_axis',(1.,0.,0.));
#23549=DIRECTION('',(0.,0.,1.));
#23550=DIRECTION('',(-0.866025403784439,0.,-0.499999999999999));
#23551=DIRECTION('',(0.866025403784439,0.,0.499999999999999));
#23552=DIRECTION('center_axis',(0.,0.,1.));
#23553=DIRECTION('ref_axis',(1.,-7.27351010247249E-15,0.));
#23554=DIRECTION('',(0.866025403784439,0.,-0.499999999999999));
#23555=DIRECTION('',(-0.866025403784439,0.,0.499999999999999));
#23556=DIRECTION('center_axis',(0.,1.,0.));
#23557=DIRECTION('ref_axis',(1.,0.,0.));
#23558=DIRECTION('',(0.,0.,-1.));
#23559=DIRECTION('center_axis',(0.,-1.,0.));
#23560=DIRECTION('ref_axis',(0.,0.,-1.));
#23561=DIRECTION('center_axis',(0.,0.,1.));
#23562=DIRECTION('ref_axis',(1.,1.11022302462528E-14,0.));
#23563=DIRECTION('center_axis',(0.,0.,-1.));
#23564=DIRECTION('ref_axis',(1.,0.,0.));
#23565=DIRECTION('center_axis',(0.,0.,1.));
#23566=DIRECTION('ref_axis',(1.,0.,0.));
#23567=DIRECTION('',(-0.707106781186549,-8.65956056235495E-17,0.707106781186546));
#23568=DIRECTION('center_axis',(0.,0.,-1.));
#23569=DIRECTION('ref_axis',(1.,0.,0.));
#23570=DIRECTION('center_axis',(0.,0.,-1.));
#23571=DIRECTION('ref_axis',(-1.,0.,0.));
#23572=DIRECTION('',(0.707106781186545,-8.6595605623549E-17,-0.70710678118655));
#23573=DIRECTION('center_axis',(0.,0.,-1.));
#23574=DIRECTION('ref_axis',(-1.,0.,0.));
#23575=DIRECTION('center_axis',(0.,0.,-1.));
#23576=DIRECTION('ref_axis',(1.,0.,0.));
#23577=DIRECTION('center_axis',(0.,0.,-1.));
#23578=DIRECTION('ref_axis',(1.,0.,0.));
#23579=DIRECTION('',(-0.707106781186545,8.6595605623549E-17,0.70710678118655));
#23580=DIRECTION('center_axis',(0.,0.,1.));
#23581=DIRECTION('ref_axis',(1.,0.,0.));
#23582=DIRECTION('center_axis',(0.,0.,1.));
#23583=DIRECTION('ref_axis',(1.,0.,0.));
#23584=DIRECTION('center_axis',(0.,0.,-1.));
#23585=DIRECTION('ref_axis',(-1.,0.,0.));
#23586=DIRECTION('center_axis',(0.,0.,1.));
#23587=DIRECTION('ref_axis',(1.,0.,0.));
#23588=DIRECTION('center_axis',(0.,0.,-1.));
#23589=DIRECTION('ref_axis',(-0.990993942369175,0.133906707029934,0.));
#23590=DIRECTION('center_axis',(0.,0.,-1.));
#23591=DIRECTION('ref_axis',(-0.990993942369175,0.133906707029935,0.));
#23592=DIRECTION('center_axis',(-0.133906707029936,-0.990993942369174,0.));
#23593=DIRECTION('ref_axis',(0.990993942369174,-0.133906707029936,0.));
#23594=DIRECTION('center_axis',(0.,0.,1.));
#23595=DIRECTION('ref_axis',(-0.990993942369175,0.133906707029936,0.));
#23596=DIRECTION('center_axis',(0.,0.,-1.));
#23597=DIRECTION('ref_axis',(-0.990993942369175,0.133906707029934,0.));
#23598=DIRECTION('center_axis',(0.,0.,-1.));
#23599=DIRECTION('ref_axis',(-0.990993942369175,0.133906707029936,0.));
#23600=DIRECTION('center_axis',(-0.133906707029936,-0.990993942369174,0.));
#23601=DIRECTION('ref_axis',(0.990993942369174,-0.133906707029936,0.));
#23602=DIRECTION('center_axis',(0.,0.,1.));
#23603=DIRECTION('ref_axis',(-0.990993942369175,0.133906707029935,0.));
#23604=DIRECTION('center_axis',(0.,0.,-1.));
#23605=DIRECTION('ref_axis',(-0.990993942369175,0.133906707029935,0.));
#23606=DIRECTION('',(0.,0.,1.));
#23607=DIRECTION('center_axis',(0.,0.,1.));
#23608=DIRECTION('ref_axis',(0.990993942369175,-0.133906707029936,0.));
#23609=DIRECTION('center_axis',(0.,0.,-1.));
#23610=DIRECTION('ref_axis',(-0.990993942369175,0.133906707029936,0.));
#23611=DIRECTION('',(0.,0.,-1.));
#23612=DIRECTION('center_axis',(0.,0.,1.));
#23613=DIRECTION('ref_axis',(0.990993942369175,-0.133906707029935,0.));
#23614=DIRECTION('center_axis',(0.,0.,-1.));
#23615=DIRECTION('ref_axis',(-0.990993942369175,0.133906707029935,0.));
#23616=DIRECTION('',(0.,0.,1.));
#23617=DIRECTION('center_axis',(0.,0.,1.));
#23618=DIRECTION('ref_axis',(-0.990993942369175,0.133906707029935,0.));
#23619=DIRECTION('',(0.,0.,1.));
#23620=DIRECTION('center_axis',(0.,0.,-1.));
#23621=DIRECTION('ref_axis',(-0.990993942369175,0.133906707029934,0.));
#23622=DIRECTION('center_axis',(0.,0.,1.));
#23623=DIRECTION('ref_axis',(-0.990993942369175,0.133906707029934,0.));
#23624=DIRECTION('',(0.,0.,1.));
#23625=DIRECTION('center_axis',(0.,0.,-1.));
#23626=DIRECTION('ref_axis',(-0.990993942369175,0.133906707029934,0.));
#23627=DIRECTION('center_axis',(0.,0.,-1.));
#23628=DIRECTION('ref_axis',(-0.990993942369175,0.133906707029936,0.));
#23629=DIRECTION('',(-0.434556986477371,-0.900644339072703,0.));
#23630=DIRECTION('',(-0.986071242772467,0.166323492559414,0.));
#23631=DIRECTION('',(0.166323492559414,0.986071242772467,0.));
#23632=DIRECTION('',(-0.461967687527403,0.886896755930804,0.));
#23633=DIRECTION('',(-0.573632924010497,0.819112488301312,0.));
#23634=DIRECTION('',(-0.909238313074883,0.41627597821246,0.));
#23635=DIRECTION('',(-0.947556814961333,0.319587362735659,0.));
#23636=DIRECTION('center_axis',(0.,0.,-1.));
#23637=DIRECTION('ref_axis',(-0.990993942369174,0.133906707029937,0.));
#23638=DIRECTION('',(0.705703477039673,-0.708507305886196,0.));
#23639=DIRECTION('',(0.923615773230652,-0.383319583949927,0.));
#23640=DIRECTION('',(0.990993942369174,-0.133906707029936,0.));
#23641=DIRECTION('',(0.885144693704452,0.465315883252282,0.));
#23642=DIRECTION('',(0.662959137150796,-0.748655583341414,0.));
#23643=DIRECTION('',(-0.691641091103085,-0.722241373155633,0.));
#23644=DIRECTION('center_axis',(0.,0.,1.));
#23645=DIRECTION('ref_axis',(0.990993942369175,-0.133906707029936,0.));
#23646=DIRECTION('center_axis',(0.,0.,-1.));
#23647=DIRECTION('ref_axis',(-0.990993942369175,0.133906707029936,0.));
#23648=DIRECTION('',(0.,0.,1.));
#23649=DIRECTION('center_axis',(0.,0.,1.));
#23650=DIRECTION('ref_axis',(0.990993942369175,-0.133906707029936,0.));
#23651=DIRECTION('',(0.,0.,1.));
#23652=DIRECTION('center_axis',(0.,0.,-1.));
#23653=DIRECTION('ref_axis',(-0.990993942369175,0.133906707029936,0.));
#23654=DIRECTION('',(0.166323492559414,0.986071242772467,0.));
#23655=DIRECTION('',(0.986071242772467,-0.166323492559414,0.));
#23656=DIRECTION('',(-0.434556986477371,-0.900644339072703,0.));
#23657=DIRECTION('',(-0.691641091103085,-0.722241373155633,0.));
#23658=DIRECTION('',(-0.639459501656208,0.768824782210871,0.));
#23659=DIRECTION('',(0.885144693704452,0.465315883252282,0.));
#23660=DIRECTION('',(0.990993942369174,-0.133906707029936,0.));
#23661=DIRECTION('',(0.923615773230652,-0.383319583949927,0.));
#23662=DIRECTION('',(0.705703477039673,-0.708507305886196,0.));
#23663=DIRECTION('center_axis',(0.,0.,-1.));
#23664=DIRECTION('ref_axis',(-0.990993942369174,0.133906707029937,0.));
#23665=DIRECTION('',(-0.947556814961333,0.319587362735659,0.));
#23666=DIRECTION('',(-0.909238313074883,0.41627597821246,0.));
#23667=DIRECTION('',(-0.573632924010497,0.819112488301312,0.));
#23668=DIRECTION('',(-0.461967687527403,0.886896755930804,0.));
#23669=DIRECTION('center_axis',(0.,0.,-1.));
#23670=DIRECTION('ref_axis',(-0.990993942369174,0.133906707029938,0.));
#23671=DIRECTION('',(0.297235194420542,0.954804293663252,0.));
#23672=DIRECTION('',(0.975502371165105,0.219988917564631,0.));
#23673=DIRECTION('',(0.678267176744562,-0.734815376098623,0.));
#23674=DIRECTION('',(-0.297235194420543,-0.954804293663252,0.));
#23675=DIRECTION('',(-0.975502371165106,-0.219988917564629,0.));
#23676=DIRECTION('',(-0.678267176744562,0.734815376098623,0.));
#23677=DIRECTION('center_axis',(0.986071242772468,-0.166323492559414,0.));
#23678=DIRECTION('ref_axis',(0.166323492559414,0.986071242772467,0.));
#23679=DIRECTION('',(-0.166323492559414,-0.986071242772467,0.));
#23680=DIRECTION('center_axis',(-0.986071242772467,0.166323492559414,0.));
#23681=DIRECTION('ref_axis',(-0.166323492559414,-0.986071242772467,0.));
#23682=DIRECTION('',(0.,0.,-1.));
#23683=DIRECTION('center_axis',(0.986071242772467,-0.166323492559414,0.));
#23684=DIRECTION('ref_axis',(-0.166323492559414,-0.986071242772467,0.));
#23685=DIRECTION('',(0.,0.,1.));
#23686=DIRECTION('center_axis',(-0.986071242772467,0.166323492559414,1.02716263700652E-30));
#23687=DIRECTION('ref_axis',(-0.166323492559414,-0.986071242772467,-1.35177217172879E-45));
#23688=DIRECTION('',(0.,0.,-1.));
#23689=DIRECTION('center_axis',(0.986071242772467,-0.166323492559414,0.));
#23690=DIRECTION('ref_axis',(-0.166323492559414,-0.986071242772467,0.));
#23691=DIRECTION('',(0.166323492559414,0.986071242772467,0.));
#23692=DIRECTION('center_axis',(0.886896755930804,0.461967687527403,0.));
#23693=DIRECTION('ref_axis',(0.,0.,-1.));
#23694=DIRECTION('',(0.,0.,1.));
#23695=DIRECTION('center_axis',(0.819112488301313,0.573632924010497,0.));
#23696=DIRECTION('ref_axis',(0.,0.,-1.));
#23697=DIRECTION('',(0.,0.,1.));
#23698=DIRECTION('center_axis',(0.41627597821246,0.909238313074883,0.));
#23699=DIRECTION('ref_axis',(0.,0.,-1.));
#23700=DIRECTION('',(0.,0.,1.));
#23701=DIRECTION('center_axis',(0.319587362735659,0.947556814961333,0.));
#23702=DIRECTION('ref_axis',(0.,0.,-1.));
#23703=DIRECTION('',(0.,0.,1.));
#23704=DIRECTION('center_axis',(0.,0.,1.));
#23705=DIRECTION('ref_axis',(-0.803690873252051,0.595047040368538,0.));
#23706=DIRECTION('',(0.,0.,1.));
#23707=DIRECTION('center_axis',(-0.708507305886196,-0.705703477039673,0.));
#23708=DIRECTION('ref_axis',(0.,0.,1.));
#23709=DIRECTION('',(0.,0.,1.));
#23710=DIRECTION('center_axis',(-0.383319583949927,-0.923615773230652,0.));
#23711=DIRECTION('ref_axis',(0.,0.,1.));
#23712=DIRECTION('',(0.,0.,1.));
#23713=DIRECTION('center_axis',(-0.133906707029936,-0.990993942369175,0.));
#23714=DIRECTION('ref_axis',(0.,0.,1.));
#23715=DIRECTION('',(0.,0.,1.));
#23716=DIRECTION('center_axis',(0.465315883252282,-0.885144693704452,0.));
#23717=DIRECTION('ref_axis',(0.885144693704452,0.465315883252282,0.));
#23718=DIRECTION('center_axis',(-0.465315883252296,0.885144693704445,-2.1507739644884E-14));
#23719=DIRECTION('ref_axis',(0.885144693704445,0.465315883252296,-7.92224047828207E-11));
#23720=DIRECTION('',(0.,0.,1.));
#23721=DIRECTION('center_axis',(0.465315883252259,-0.885144693704465,-2.38928391774824E-14));
#23722=DIRECTION('ref_axis',(0.885144693704465,0.465315883252258,-1.11680359097547E-11));
#23723=DIRECTION('',(-0.885144693704452,-0.465315883252282,0.));
#23724=DIRECTION('',(0.885144693704452,0.465315883252282,0.));
#23725=DIRECTION('center_axis',(-0.465315883252314,0.885144693704436,-5.15404751531186E-14));
#23726=DIRECTION('ref_axis',(0.885144693704436,0.465315883252314,7.55878627128317E-11));
#23727=DIRECTION('',(0.,0.,1.));
#23728=DIRECTION('center_axis',(0.465315883252266,-0.885144693704461,-1.83477419639032E-14));
#23729=DIRECTION('ref_axis',(0.885144693704461,0.465315883252266,-5.12289412685469E-12));
#23730=DIRECTION('center_axis',(-0.722241373155633,0.691641091103085,0.));
#23731=DIRECTION('ref_axis',(0.,0.,1.));
#23732=DIRECTION('',(0.,0.,1.));
#23733=DIRECTION('center_axis',(0.722241373155643,-0.691641091103075,-1.34943523468737E-15));
#23734=DIRECTION('ref_axis',(0.691641091103075,0.722241373155643,-2.2903875502264E-10));
#23735=DIRECTION('',(0.,0.,1.));
#23736=DIRECTION('center_axis',(-0.72224137315561,0.691641091103109,3.34490341472713E-14));
#23737=DIRECTION('ref_axis',(0.691641091103109,0.72224137315561,-4.63418217506663E-10));
#23738=DIRECTION('',(0.,0.,1.));
#23739=DIRECTION('center_axis',(0.722241373155679,-0.691641091103037,7.1290365707807E-14));
#23740=DIRECTION('ref_axis',(0.691641091103036,0.722241373155679,4.52709546294639E-10));
#23741=DIRECTION('',(-0.691641091103085,-0.722241373155633,0.));
#23742=DIRECTION('',(0.691641091103085,0.722241373155633,0.));
#23743=DIRECTION('center_axis',(-0.722241373155636,0.691641091103082,-2.46271930330266E-14));
#23744=DIRECTION('ref_axis',(0.691641091103082,0.722241373155636,4.41696351613122E-10));
#23745=DIRECTION('center_axis',(-0.900644339072703,0.434556986477371,0.));
#23746=DIRECTION('ref_axis',(0.,0.,1.));
#23747=DIRECTION('',(0.,0.,-1.));
#23748=DIRECTION('center_axis',(0.900644339072708,-0.434556986477361,3.87104187789662E-16));
#23749=DIRECTION('ref_axis',(0.434556986477361,0.900644339072708,-1.76194029248825E-11));
#23750=DIRECTION('',(0.434556986477371,0.900644339072703,0.));
#23751=DIRECTION('',(-0.434556986477371,-0.900644339072703,0.));
#23752=DIRECTION('center_axis',(-0.900644339072692,0.434556986477393,2.41940117368536E-14));
#23753=DIRECTION('ref_axis',(0.434556986477393,0.900644339072692,9.15800115337473E-12));
#23754=DIRECTION('',(0.,0.,-1.));
#23755=DIRECTION('center_axis',(0.900644339072707,-0.434556986477363,1.7371300427058E-14));
#23756=DIRECTION('ref_axis',(0.434556986477363,0.900644339072707,-3.82265683540711E-11));
#23757=DIRECTION('center_axis',(-0.900644339072698,0.434556986477381,1.01614849294736E-14));
#23758=DIRECTION('ref_axis',(0.434556986477381,0.900644339072698,6.73661852370467E-11));
#23759=DIRECTION('center_axis',(0.,0.,-1.));
#23760=DIRECTION('ref_axis',(-0.990993942369175,0.133906707029936,0.));
#23761=DIRECTION('',(-0.662959137150796,0.748655583341414,0.));
#23762=DIRECTION('center_axis',(0.748655583341414,0.662959137150796,0.));
#23763=DIRECTION('ref_axis',(0.,0.,-1.));
#23764=DIRECTION('',(-0.662959137150796,0.748655583341414,0.));
#23765=DIRECTION('',(0.662959137150796,-0.748655583341414,0.));
#23766=DIRECTION('center_axis',(-0.768824782210871,-0.639459501656208,0.));
#23767=DIRECTION('ref_axis',(0.,0.,1.));
#23768=DIRECTION('',(-0.639459501656208,0.768824782210871,0.));
#23769=DIRECTION('',(0.639459501656208,-0.768824782210871,0.));
#23770=DIRECTION('center_axis',(0.,0.,-1.));
#23771=DIRECTION('ref_axis',(-0.990993942369175,0.133906707029936,0.));
#23772=DIRECTION('',(0.639459501656208,-0.768824782210871,0.));
#23773=DIRECTION('center_axis',(-0.639459501656208,0.768824782210872,0.));
#23774=DIRECTION('ref_axis',(0.768824782210872,0.639459501656208,0.));
#23775=DIRECTION('center_axis',(0.639459501656208,-0.768824782210871,0.));
#23776=DIRECTION('ref_axis',(-0.768824782210871,-0.639459501656208,0.));
#23777=DIRECTION('center_axis',(-0.662959137150795,0.748655583341415,0.));
#23778=DIRECTION('ref_axis',(0.748655583341415,0.662959137150795,0.));
#23779=DIRECTION('center_axis',(0.662959137150795,-0.748655583341415,0.));
#23780=DIRECTION('ref_axis',(-0.748655583341415,-0.662959137150795,0.));
#23781=DIRECTION('center_axis',(0.,0.,1.));
#23782=DIRECTION('ref_axis',(-0.133906707029936,-0.990993942369175,0.));
#23783=DIRECTION('',(-0.986071242772467,0.166323492559414,0.));
#23784=DIRECTION('center_axis',(-0.166323492559414,-0.986071242772468,0.));
#23785=DIRECTION('ref_axis',(0.,0.,1.));
#23786=DIRECTION('',(0.986071242772467,-0.166323492559414,0.));
#23787=DIRECTION('',(-0.986071242772467,0.166323492559414,0.));
#23788=DIRECTION('center_axis',(0.166323492559414,0.986071242772467,0.));
#23789=DIRECTION('ref_axis',(0.,0.,-1.));
#23790=DIRECTION('',(-0.986071242772467,0.166323492559414,0.));
#23791=DIRECTION('',(0.986071242772467,-0.166323492559414,0.));
#23792=DIRECTION('center_axis',(0.,0.,-1.));
#23793=DIRECTION('ref_axis',(-0.990993942369175,0.133906707029936,0.));
#23794=DIRECTION('',(0.986071242772467,-0.166323492559414,0.));
#23795=DIRECTION('center_axis',(0.986071242772468,-0.166323492559414,0.));
#23796=DIRECTION('ref_axis',(-0.166323492559414,-0.986071242772467,0.));
#23797=DIRECTION('center_axis',(0.986071242772467,-0.166323492559414,0.));
#23798=DIRECTION('ref_axis',(-0.166323492559414,-0.986071242772467,0.));
#23799=DIRECTION('center_axis',(0.986071242772467,-0.166323492559414,0.));
#23800=DIRECTION('ref_axis',(-0.166323492559414,-0.986071242772467,0.));
#23801=DIRECTION('center_axis',(-0.986071242772467,0.166323492559414,0.));
#23802=DIRECTION('ref_axis',(0.166323492559414,0.986071242772467,0.));
#23803=DIRECTION('center_axis',(0.,0.,-1.));
#23804=DIRECTION('ref_axis',(-0.990993942369175,0.133906707029936,0.));
#23805=DIRECTION('center_axis',(0.,0.,-1.));
#23806=DIRECTION('ref_axis',(-0.990993942369175,0.133906707029936,0.));
#23807=DIRECTION('center_axis',(0.219988917564632,-0.975502371165105,0.));
#23808=DIRECTION('ref_axis',(0.975502371165105,0.219988917564631,0.));
#23809=DIRECTION('',(0.,0.,1.));
#23810=DIRECTION('',(-0.975502371165105,-0.219988917564631,0.));
#23811=DIRECTION('',(0.,0.,1.));
#23812=DIRECTION('center_axis',(0.954804293663253,-0.297235194420542,0.));
#23813=DIRECTION('ref_axis',(0.297235194420542,0.954804293663252,0.));
#23814=DIRECTION('',(0.,0.,1.));
#23815=DIRECTION('',(-0.297235194420542,-0.954804293663252,0.));
#23816=DIRECTION('center_axis',(0.734815376098623,0.678267176744562,0.));
#23817=DIRECTION('ref_axis',(0.,0.,-1.));
#23818=DIRECTION('',(0.,0.,1.));
#23819=DIRECTION('',(0.678267176744562,-0.734815376098623,0.));
#23820=DIRECTION('center_axis',(-0.219988917564628,0.975502371165105,0.));
#23821=DIRECTION('ref_axis',(0.,0.,1.));
#23822=DIRECTION('',(0.,0.,1.));
#23823=DIRECTION('',(0.975502371165106,0.219988917564629,0.));
#23824=DIRECTION('center_axis',(-0.954804293663252,0.297235194420544,0.));
#23825=DIRECTION('ref_axis',(0.,0.,1.));
#23826=DIRECTION('',(0.,0.,1.));
#23827=DIRECTION('',(0.297235194420543,0.954804293663252,0.));
#23828=DIRECTION('center_axis',(-0.734815376098623,-0.678267176744562,0.));
#23829=DIRECTION('ref_axis',(0.,0.,1.));
#23830=DIRECTION('',(-0.678267176744562,0.734815376098623,0.));
#23831=DIRECTION('center_axis',(0.,0.,-1.));
#23832=DIRECTION('ref_axis',(-0.990993942369175,0.133906707029936,0.));
#23833=DIRECTION('',(-0.975502371165105,-0.219988917564628,0.));
#23834=DIRECTION('',(-0.297235194420543,-0.954804293663252,0.));
#23835=DIRECTION('',(0.678267176744562,-0.734815376098623,0.));
#23836=DIRECTION('',(0.975502371165105,0.219988917564631,0.));
#23837=DIRECTION('',(0.297235194420542,0.954804293663252,0.));
#23838=DIRECTION('',(-0.678267176744562,0.734815376098623,0.));
#23839=DIRECTION('center_axis',(-0.297235194420542,-0.954804293663253,0.));
#23840=DIRECTION('ref_axis',(-0.954804293663252,0.297235194420542,0.));
#23841=DIRECTION('center_axis',(-0.734815376098582,-0.678267176744606,5.08035781491937E-14));
#23842=DIRECTION('ref_axis',(0.678267176744606,-0.734815376098582,-3.83211898500117E-12));
#23843=DIRECTION('center_axis',(-0.219988917564645,0.975502371165102,5.18008130528868E-14));
#23844=DIRECTION('ref_axis',(0.975502371165102,0.219988917564645,-8.45195070037509E-12));
#23845=DIRECTION('center_axis',(0.678267176744561,-0.734815376098624,0.));
#23846=DIRECTION('ref_axis',(-0.734815376098624,-0.678267176744561,0.));
#23847=DIRECTION('center_axis',(-0.954804293663248,0.297235194420558,-1.28532498698092E-14));
#23848=DIRECTION('ref_axis',(0.297235194420558,0.954804293663248,-1.26871517833745E-11));
#23849=DIRECTION('center_axis',(-0.975502371165106,-0.219988917564627,0.));
#23850=DIRECTION('ref_axis',(-0.219988917564627,0.975502371165106,0.));
#23851=DIRECTION('center_axis',(-0.954804293663331,0.297235194420291,2.31967918986522E-13));
#23852=DIRECTION('ref_axis',(0.297235194420291,0.954804293663331,5.5906824425949E-12));
#23853=DIRECTION('center_axis',(0.975502371165106,0.219988917564627,0.));
#23854=DIRECTION('ref_axis',(0.219988917564627,-0.975502371165106,0.));
#23855=DIRECTION('center_axis',(-0.734815376098563,-0.678267176744628,-1.56233468245057E-14));
#23856=DIRECTION('ref_axis',(0.678267176744628,-0.734815376098563,2.56800988528237E-12));
#23857=DIRECTION('center_axis',(-0.678267176744561,0.734815376098624,0.));
#23858=DIRECTION('ref_axis',(0.734815376098624,0.678267176744561,0.));
#23859=DIRECTION('center_axis',(-0.219988917564712,0.975502371165087,1.20748526255343E-13));
#23860=DIRECTION('ref_axis',(0.975502371165087,0.219988917564712,-8.28276908751904E-12));
#23861=DIRECTION('center_axis',(0.297235194420542,0.954804293663253,0.));
#23862=DIRECTION('ref_axis',(0.954804293663252,-0.297235194420542,0.));
#23863=DIRECTION('center_axis',(0.,0.,1.));
#23864=DIRECTION('ref_axis',(0.990993942369174,-0.133906707029938,0.));
#23865=DIRECTION('',(0.,0.,1.));
#23866=DIRECTION('center_axis',(0.,0.,1.));
#23867=DIRECTION('ref_axis',(1.,0.,0.));
#23868=DIRECTION('center_axis',(0.,0.,1.));
#23869=DIRECTION('ref_axis',(1.,0.,0.));
#23870=DIRECTION('center_axis',(0.,0.,-1.));
#23871=DIRECTION('ref_axis',(-0.999820197862873,0.0189623823779183,0.));
#23872=DIRECTION('',(0.,0.,-1.));
#23873=DIRECTION('center_axis',(0.,0.,1.));
#23874=DIRECTION('ref_axis',(0.999820197862873,-0.0189623823779183,0.));
#23875=DIRECTION('center_axis',(0.39446700523415,0.918910105386594,0.));
#23876=DIRECTION('ref_axis',(0.,0.,-1.));
#23877=DIRECTION('',(0.918910105386594,-0.39446700523415,0.));
#23878=DIRECTION('',(0.,0.,-1.));
#23879=DIRECTION('',(0.918910105386594,-0.39446700523415,0.));
#23880=DIRECTION('',(0.,0.,-1.));
#23881=DIRECTION('center_axis',(0.,0.,-1.));
#23882=DIRECTION('ref_axis',(-0.999820197862872,0.0189623823779211,0.));
#23883=DIRECTION('center_axis',(0.,0.,1.));
#23884=DIRECTION('ref_axis',(0.999820197862872,-0.0189623823779211,0.));
#23885=DIRECTION('',(0.,0.,-1.));
#23886=DIRECTION('center_axis',(0.,0.,1.));
#23887=DIRECTION('ref_axis',(0.999820197862872,-0.0189623823779211,0.));
#23888=DIRECTION('center_axis',(-0.399400362728205,-0.91677660869624,0.));
#23889=DIRECTION('ref_axis',(-0.91677660869624,0.399400362728205,0.));
#23890=DIRECTION('',(-0.91677660869624,0.399400362728205,0.));
#23891=DIRECTION('',(-0.91677660869624,0.399400362728205,0.));
#23892=DIRECTION('',(0.,0.,-1.));
#23893=DIRECTION('center_axis',(-0.844295148658605,-0.535878439528541,0.));
#23894=DIRECTION('ref_axis',(-0.535878439528541,0.844295148658605,0.));
#23895=DIRECTION('',(-0.535878439528541,0.844295148658605,0.));
#23896=DIRECTION('',(-0.535878439528541,0.844295148658605,0.));
#23897=DIRECTION('',(0.,0.,-1.));
#23898=DIRECTION('center_axis',(0.213055394807629,-0.977040121358056,0.));
#23899=DIRECTION('ref_axis',(0.,0.,-1.));
#23900=DIRECTION('',(-0.977040121358056,-0.213055394807629,0.));
#23901=DIRECTION('',(-0.977040121358056,-0.213055394807629,0.));
#23902=DIRECTION('',(0.,0.,-1.));
#23903=DIRECTION('center_axis',(-0.91677660869624,0.399400362728203,0.));
#23904=DIRECTION('ref_axis',(0.,0.,1.));
#23905=DIRECTION('',(0.399400362728203,0.91677660869624,0.));
#23906=DIRECTION('',(0.399400362728203,0.91677660869624,0.));
#23907=DIRECTION('',(0.,0.,-1.));
#23908=DIRECTION('center_axis',(-0.38850791323187,-0.921445387071973,0.));
#23909=DIRECTION('ref_axis',(-0.921445387071973,0.38850791323187,0.));
#23910=DIRECTION('',(-0.921445387071973,0.38850791323187,0.));
#23911=DIRECTION('',(-0.921445387071973,0.38850791323187,0.));
#23912=DIRECTION('',(0.,0.,-1.));
#23913=DIRECTION('center_axis',(0.213055394807629,-0.977040121358056,0.));
#23914=DIRECTION('ref_axis',(0.,0.,-1.));
#23915=DIRECTION('',(-0.977040121358056,-0.213055394807629,0.));
#23916=DIRECTION('',(-0.977040121358056,-0.213055394807629,0.));
#23917=DIRECTION('',(0.,0.,-1.));
#23918=DIRECTION('center_axis',(-0.91677660869624,0.399400362728203,0.));
#23919=DIRECTION('ref_axis',(0.,0.,1.));
#23920=DIRECTION('',(0.399400362728203,0.91677660869624,0.));
#23921=DIRECTION('',(0.399400362728203,0.91677660869624,0.));
#23922=DIRECTION('',(0.,0.,-1.));
#23923=DIRECTION('center_axis',(-0.388507913231866,-0.921445387071974,0.));
#23924=DIRECTION('ref_axis',(-0.921445387071975,0.388507913231866,0.));
#23925=DIRECTION('',(-0.921445387071974,0.388507913231866,0.));
#23926=DIRECTION('',(-0.921445387071974,0.388507913231866,0.));
#23927=DIRECTION('',(0.,0.,-1.));
#23928=DIRECTION('center_axis',(0.213055394807629,-0.977040121358056,0.));
#23929=DIRECTION('ref_axis',(0.,0.,-1.));
#23930=DIRECTION('',(-0.977040121358056,-0.213055394807629,0.));
#23931=DIRECTION('',(-0.977040121358056,-0.213055394807629,0.));
#23932=DIRECTION('',(0.,0.,-1.));
#23933=DIRECTION('center_axis',(-0.91677660869624,0.399400362728203,0.));
#23934=DIRECTION('ref_axis',(0.,0.,1.));
#23935=DIRECTION('',(0.399400362728203,0.91677660869624,0.));
#23936=DIRECTION('',(0.399400362728203,0.91677660869624,0.));
#23937=DIRECTION('',(0.,0.,-1.));
#23938=DIRECTION('center_axis',(-0.38850791323187,-0.921445387071973,0.));
#23939=DIRECTION('ref_axis',(-0.921445387071973,0.38850791323187,0.));
#23940=DIRECTION('',(-0.921445387071973,0.38850791323187,0.));
#23941=DIRECTION('',(-0.921445387071973,0.38850791323187,0.));
#23942=DIRECTION('',(0.,0.,-1.));
#23943=DIRECTION('center_axis',(0.213055394807629,-0.977040121358056,0.));
#23944=DIRECTION('ref_axis',(0.,0.,-1.));
#23945=DIRECTION('',(-0.977040121358056,-0.213055394807629,0.));
#23946=DIRECTION('',(-0.977040121358056,-0.213055394807629,0.));
#23947=DIRECTION('',(0.,0.,-1.));
#23948=DIRECTION('center_axis',(-0.91677660869624,0.399400362728203,0.));
#23949=DIRECTION('ref_axis',(0.,0.,1.));
#23950=DIRECTION('',(0.399400362728203,0.91677660869624,0.));
#23951=DIRECTION('',(0.399400362728203,0.91677660869624,0.));
#23952=DIRECTION('',(0.,0.,-1.));
#23953=DIRECTION('center_axis',(-0.38850791323187,-0.921445387071973,0.));
#23954=DIRECTION('ref_axis',(-0.921445387071973,0.38850791323187,0.));
#23955=DIRECTION('',(-0.921445387071973,0.38850791323187,0.));
#23956=DIRECTION('',(-0.921445387071973,0.38850791323187,0.));
#23957=DIRECTION('',(0.,0.,-1.));
#23958=DIRECTION('center_axis',(0.213055394807629,-0.977040121358056,0.));
#23959=DIRECTION('ref_axis',(0.,0.,-1.));
#23960=DIRECTION('',(-0.977040121358056,-0.213055394807629,0.));
#23961=DIRECTION('',(-0.977040121358056,-0.213055394807629,0.));
#23962=DIRECTION('',(0.,0.,-1.));
#23963=DIRECTION('center_axis',(-0.916776608696241,0.399400362728203,0.));
#23964=DIRECTION('ref_axis',(0.,0.,1.));
#23965=DIRECTION('',(0.399400362728203,0.916776608696241,0.));
#23966=DIRECTION('',(0.399400362728203,0.916776608696241,0.));
#23967=DIRECTION('',(0.,0.,-1.));
#23968=DIRECTION('center_axis',(-0.388507913231868,-0.921445387071974,0.));
#23969=DIRECTION('ref_axis',(-0.921445387071974,0.388507913231868,0.));
#23970=DIRECTION('',(-0.921445387071974,0.388507913231868,0.));
#23971=DIRECTION('',(-0.921445387071974,0.388507913231868,0.));
#23972=DIRECTION('',(0.,0.,-1.));
#23973=DIRECTION('center_axis',(0.213055394807629,-0.977040121358056,0.));
#23974=DIRECTION('ref_axis',(0.,0.,-1.));
#23975=DIRECTION('',(-0.977040121358056,-0.213055394807629,0.));
#23976=DIRECTION('',(-0.977040121358056,-0.213055394807629,0.));
#23977=DIRECTION('',(0.,0.,-1.));
#23978=DIRECTION('center_axis',(-0.91677660869624,0.399400362728203,0.));
#23979=DIRECTION('ref_axis',(0.,0.,1.));
#23980=DIRECTION('',(0.399400362728203,0.91677660869624,0.));
#23981=DIRECTION('',(0.399400362728203,0.91677660869624,0.));
#23982=DIRECTION('',(0.,0.,-1.));
#23983=DIRECTION('center_axis',(-0.38850791323187,-0.921445387071973,0.));
#23984=DIRECTION('ref_axis',(-0.921445387071973,0.38850791323187,0.));
#23985=DIRECTION('',(-0.921445387071973,0.38850791323187,0.));
#23986=DIRECTION('',(-0.921445387071973,0.38850791323187,0.));
#23987=DIRECTION('',(0.,0.,-1.));
#23988=DIRECTION('center_axis',(0.213055394807629,-0.977040121358056,0.));
#23989=DIRECTION('ref_axis',(0.,0.,-1.));
#23990=DIRECTION('',(-0.977040121358056,-0.213055394807629,0.));
#23991=DIRECTION('',(-0.977040121358056,-0.213055394807629,0.));
#23992=DIRECTION('',(0.,0.,-1.));
#23993=DIRECTION('center_axis',(-0.916776608696241,0.399400362728203,0.));
#23994=DIRECTION('ref_axis',(0.,0.,1.));
#23995=DIRECTION('',(0.399400362728203,0.916776608696241,0.));
#23996=DIRECTION('',(0.399400362728203,0.916776608696241,0.));
#23997=DIRECTION('',(0.,0.,-1.));
#23998=DIRECTION('center_axis',(-0.388507913231866,-0.921445387071974,0.));
#23999=DIRECTION('ref_axis',(-0.921445387071975,0.388507913231866,0.));
#24000=DIRECTION('',(-0.921445387071974,0.388507913231866,0.));
#24001=DIRECTION('',(-0.921445387071974,0.388507913231866,0.));
#24002=DIRECTION('',(0.,0.,-1.));
#24003=DIRECTION('center_axis',(0.21305539480763,-0.977040121358056,0.));
#24004=DIRECTION('ref_axis',(0.,0.,-1.));
#24005=DIRECTION('',(-0.977040121358056,-0.21305539480763,0.));
#24006=DIRECTION('',(-0.977040121358056,-0.21305539480763,0.));
#24007=DIRECTION('',(0.,0.,-1.));
#24008=DIRECTION('center_axis',(-0.916776608696241,0.399400362728203,0.));
#24009=DIRECTION('ref_axis',(0.,0.,1.));
#24010=DIRECTION('',(0.399400362728203,0.916776608696241,0.));
#24011=DIRECTION('',(0.399400362728203,0.916776608696241,0.));
#24012=DIRECTION('',(0.,0.,-1.));
#24013=DIRECTION('center_axis',(-0.388507913231866,-0.921445387071974,0.));
#24014=DIRECTION('ref_axis',(-0.921445387071975,0.388507913231866,0.));
#24015=DIRECTION('',(-0.921445387071974,0.388507913231866,0.));
#24016=DIRECTION('',(-0.921445387071974,0.388507913231866,0.));
#24017=DIRECTION('',(0.,0.,-1.));
#24018=DIRECTION('center_axis',(0.21305539480763,-0.977040121358056,0.));
#24019=DIRECTION('ref_axis',(0.,0.,-1.));
#24020=DIRECTION('',(-0.977040121358056,-0.21305539480763,0.));
#24021=DIRECTION('',(-0.977040121358056,-0.21305539480763,0.));
#24022=DIRECTION('',(0.,0.,-1.));
#24023=DIRECTION('center_axis',(-0.91677660869624,0.399400362728203,0.));
#24024=DIRECTION('ref_axis',(0.,0.,1.));
#24025=DIRECTION('',(0.399400362728203,0.91677660869624,0.));
#24026=DIRECTION('',(0.399400362728203,0.91677660869624,0.));
#24027=DIRECTION('',(0.,0.,-1.));
#24028=DIRECTION('center_axis',(-0.388507913231866,-0.921445387071974,0.));
#24029=DIRECTION('ref_axis',(-0.921445387071975,0.388507913231866,0.));
#24030=DIRECTION('',(-0.921445387071974,0.388507913231866,0.));
#24031=DIRECTION('',(-0.921445387071974,0.388507913231866,0.));
#24032=DIRECTION('',(0.,0.,-1.));
#24033=DIRECTION('center_axis',(0.213055394807629,-0.977040121358056,0.));
#24034=DIRECTION('ref_axis',(0.,0.,-1.));
#24035=DIRECTION('',(-0.977040121358056,-0.213055394807629,0.));
#24036=DIRECTION('',(-0.977040121358056,-0.213055394807629,0.));
#24037=DIRECTION('',(0.,0.,-1.));
#24038=DIRECTION('center_axis',(-0.91677660869624,0.399400362728203,0.));
#24039=DIRECTION('ref_axis',(0.,0.,1.));
#24040=DIRECTION('',(0.399400362728203,0.91677660869624,0.));
#24041=DIRECTION('',(0.399400362728203,0.91677660869624,0.));
#24042=DIRECTION('',(0.,0.,-1.));
#24043=DIRECTION('center_axis',(-0.388507913231873,-0.921445387071972,0.));
#24044=DIRECTION('ref_axis',(-0.921445387071971,0.388507913231873,0.));
#24045=DIRECTION('',(-0.921445387071971,0.388507913231873,0.));
#24046=DIRECTION('',(-0.921445387071971,0.388507913231873,0.));
#24047=DIRECTION('',(0.,0.,-1.));
#24048=DIRECTION('center_axis',(0.213055394807629,-0.977040121358056,0.));
#24049=DIRECTION('ref_axis',(0.,0.,-1.));
#24050=DIRECTION('',(-0.977040121358056,-0.213055394807629,0.));
#24051=DIRECTION('',(-0.977040121358056,-0.213055394807629,0.));
#24052=DIRECTION('',(0.,0.,-1.));
#24053=DIRECTION('center_axis',(-0.916776608696241,0.399400362728203,0.));
#24054=DIRECTION('ref_axis',(0.,0.,1.));
#24055=DIRECTION('',(0.399400362728203,0.916776608696241,0.));
#24056=DIRECTION('',(0.399400362728203,0.916776608696241,0.));
#24057=DIRECTION('',(0.,0.,-1.));
#24058=DIRECTION('center_axis',(-0.388507913231871,-0.921445387071973,0.));
#24059=DIRECTION('ref_axis',(-0.921445387071973,0.388507913231871,0.));
#24060=DIRECTION('',(-0.921445387071973,0.388507913231871,0.));
#24061=DIRECTION('',(-0.921445387071973,0.388507913231871,0.));
#24062=DIRECTION('',(0.,0.,-1.));
#24063=DIRECTION('center_axis',(0.213055394807631,-0.977040121358056,0.));
#24064=DIRECTION('ref_axis',(0.,0.,-1.));
#24065=DIRECTION('',(-0.977040121358056,-0.213055394807631,0.));
#24066=DIRECTION('',(-0.977040121358056,-0.213055394807631,0.));
#24067=DIRECTION('',(0.,0.,-1.));
#24068=DIRECTION('center_axis',(-0.916776608696241,0.399400362728203,0.));
#24069=DIRECTION('ref_axis',(0.,0.,1.));
#24070=DIRECTION('',(0.399400362728203,0.916776608696241,0.));
#24071=DIRECTION('',(0.399400362728203,0.916776608696241,0.));
#24072=DIRECTION('',(0.,0.,-1.));
#24073=DIRECTION('center_axis',(-0.436416285895279,-0.899744866840245,0.));
#24074=DIRECTION('ref_axis',(-0.899744866840245,0.436416285895279,0.));
#24075=DIRECTION('',(-0.899744866840245,0.436416285895278,0.));
#24076=DIRECTION('',(-0.899744866840245,0.436416285895278,0.));
#24077=DIRECTION('',(0.,0.,-1.));
#24078=DIRECTION('center_axis',(0.,0.,-1.));
#24079=DIRECTION('ref_axis',(-0.999820197862872,0.0189623823779216,0.));
#24080=DIRECTION('center_axis',(0.,0.,1.));
#24081=DIRECTION('ref_axis',(-0.999820197862872,0.0189623823779216,0.));
#24082=DIRECTION('center_axis',(0.,0.,1.));
#24083=DIRECTION('ref_axis',(-0.999820197862872,0.0189623823779216,0.));
#24084=DIRECTION('',(0.,0.,-1.));
#24085=DIRECTION('center_axis',(0.399400362728205,0.91677660869624,0.));
#24086=DIRECTION('ref_axis',(0.,0.,-1.));
#24087=DIRECTION('',(0.91677660869624,-0.399400362728205,0.));
#24088=DIRECTION('',(0.91677660869624,-0.399400362728205,0.));
#24089=DIRECTION('',(0.,0.,-1.));
#24090=DIRECTION('center_axis',(0.740794344427866,0.671731895374701,0.));
#24091=DIRECTION('ref_axis',(0.,0.,-1.));
#24092=DIRECTION('',(0.671731895374701,-0.740794344427866,0.));
#24093=DIRECTION('',(0.671731895374701,-0.740794344427866,0.));
#24094=DIRECTION('center_axis',(0.,0.,1.));
#24095=DIRECTION('ref_axis',(0.999820197862872,-0.018962382377922,0.));
#24096=DIRECTION('center_axis',(0.,0.,1.));
#24097=DIRECTION('ref_axis',(0.999820197862872,-0.018962382377922,0.));
#24098=DIRECTION('center_axis',(0.,0.,1.));
#24099=DIRECTION('ref_axis',(1.,0.,0.));
#24100=DIRECTION('axis',(0.,0.,1.));
#24101=DIRECTION('refdir',(1.,0.,0.));
#24102=DIRECTION('center_axis',(0.,0.,-1.));
#24103=DIRECTION('ref_axis',(-1.,0.,0.));
#24104=DIRECTION('center_axis',(0.,0.,1.));
#24105=DIRECTION('ref_axis',(1.,0.,0.));
#24106=DIRECTION('',(0.,0.,-1.));
#24107=DIRECTION('center_axis',(0.,0.,-1.));
#24108=DIRECTION('ref_axis',(-1.,0.,0.));
#24109=DIRECTION('center_axis',(-0.999428214444506,-0.033811893946752,0.));
#24110=DIRECTION('ref_axis',(-0.033811893946752,0.999428214444506,0.));
#24111=DIRECTION('',(0.033811893946752,-0.999428214444506,0.));
#24112=DIRECTION('',(0.,0.,1.));
#24113=DIRECTION('',(0.033811893946752,-0.999428214444506,0.));
#24114=DIRECTION('',(0.,0.,1.));
#24115=DIRECTION('center_axis',(0.,0.,1.));
#24116=DIRECTION('ref_axis',(0.999428214444506,0.0338118939467526,0.));
#24117=DIRECTION('center_axis',(0.,0.,-1.));
#24118=DIRECTION('ref_axis',(0.999428214444506,0.0338118939467526,0.));
#24119=DIRECTION('',(0.,0.,1.));
#24120=DIRECTION('center_axis',(0.,0.,-1.));
#24121=DIRECTION('ref_axis',(0.999428214444506,0.0338118939467526,0.));
#24122=DIRECTION('center_axis',(0.999428214444506,0.0338118939467537,0.));
#24123=DIRECTION('ref_axis',(0.,0.,-1.));
#24124=DIRECTION('',(-0.0338118939467537,0.999428214444506,0.));
#24125=DIRECTION('',(-0.0338118939467537,0.999428214444506,0.));
#24126=DIRECTION('',(0.,0.,1.));
#24127=DIRECTION('center_axis',(0.175442327597817,-0.984489710300245,0.));
#24128=DIRECTION('ref_axis',(0.984489710300245,0.175442327597816,0.));
#24129=DIRECTION('',(0.984489710300245,0.175442327597816,0.));
#24130=DIRECTION('',(0.984489710300248,0.1754423275978,0.));
#24131=DIRECTION('',(0.,0.,1.));
#24132=DIRECTION('center_axis',(0.314024880544539,-0.949414753624036,0.));
#24133=DIRECTION('ref_axis',(0.949414753624036,0.314024880544539,0.));
#24134=DIRECTION('',(0.949414753624036,0.314024880544539,0.));
#24135=DIRECTION('',(0.949414753624036,0.314024880544539,0.));
#24136=DIRECTION('',(0.,0.,1.));
#24137=DIRECTION('center_axis',(0.999428214444506,0.033811893946752,0.));
#24138=DIRECTION('ref_axis',(0.,0.,-1.));
#24139=DIRECTION('',(-0.033811893946752,0.999428214444506,0.));
#24140=DIRECTION('',(-0.033811893946752,0.999428214444506,0.));
#24141=DIRECTION('',(0.,0.,1.));
#24142=DIRECTION('center_axis',(0.,0.,1.));
#24143=DIRECTION('ref_axis',(0.999428214444506,0.0338118939467424,0.));
#24144=DIRECTION('center_axis',(0.,0.,-1.));
#24145=DIRECTION('ref_axis',(0.999428214444506,0.0338118939467424,0.));
#24146=DIRECTION('center_axis',(0.,0.,-1.));
#24147=DIRECTION('ref_axis',(0.999428214444506,0.0338118939467424,0.));
#24148=DIRECTION('',(0.,0.,1.));
#24149=DIRECTION('center_axis',(-0.40290063302029,0.915243727054084,0.));
#24150=DIRECTION('ref_axis',(0.,0.,1.));
#24151=DIRECTION('',(-0.915243727054084,-0.402900633020289,0.));
#24152=DIRECTION('',(-0.915243727054084,-0.402900633020289,0.));
#24153=DIRECTION('',(0.,0.,1.));
#24154=DIRECTION('center_axis',(-0.702321846847344,0.711859553171084,0.));
#24155=DIRECTION('ref_axis',(0.,0.,1.));
#24156=DIRECTION('',(-0.711859553171084,-0.702321846847344,0.));
#24157=DIRECTION('',(-0.711859553171084,-0.702321846847344,0.));
#24158=DIRECTION('',(0.,0.,1.));
#24159=DIRECTION('center_axis',(-0.033811893946752,0.999428214444506,0.));
#24160=DIRECTION('ref_axis',(-0.999428214444506,-0.033811893946752,0.));
#24161=DIRECTION('',(-0.999428214444506,-0.033811893946752,0.));
#24162=DIRECTION('',(-0.999428214444506,-0.033811893946752,0.));
#24163=DIRECTION('',(0.,0.,1.));
#24164=DIRECTION('center_axis',(0.,0.,1.));
#24165=DIRECTION('ref_axis',(0.999428214444506,0.0338118939467518,0.));
#24166=DIRECTION('center_axis',(0.,0.,-1.));
#24167=DIRECTION('ref_axis',(0.999428214444506,0.0338118939467518,0.));
#24168=DIRECTION('center_axis',(0.,0.,-1.));
#24169=DIRECTION('ref_axis',(0.999428214444506,0.0338118939467518,0.));
#24170=DIRECTION('center_axis',(0.,0.,1.));
#24171=DIRECTION('ref_axis',(0.033811893946752,-0.999428214444506,0.));
#24172=DIRECTION('center_axis',(0.,0.,1.));
#24173=DIRECTION('ref_axis',(0.033811893946752,-0.999428214444506,0.));
#24174=DIRECTION('',(0.,0.,1.));
#24175=DIRECTION('',(1.,0.,0.));
#24176=DIRECTION('',(0.,0.,1.));
#24177=DIRECTION('',(1.,0.,0.));
#24178=DIRECTION('',(0.,0.,1.));
#24179=DIRECTION('',(1.,0.,0.));
#24180=DIRECTION('',(0.,0.,1.));
#24181=DIRECTION('',(1.,0.,0.));
#24182=DIRECTION('',(0.,0.,1.));
#24183=DIRECTION('',(1.,0.,0.));
#24184=DIRECTION('',(0.,0.,1.));
#24185=DIRECTION('',(1.,0.,0.));
#24186=DIRECTION('',(0.,0.,1.));
#24187=DIRECTION('',(1.,0.,0.));
#24188=DIRECTION('',(0.,0.,1.));
#24189=DIRECTION('',(1.,0.,0.));
#24190=DIRECTION('',(0.,0.,1.));
#24191=DIRECTION('',(1.,0.,0.));
#24192=DIRECTION('',(0.,0.,1.));
#24193=DIRECTION('',(1.,0.,0.));
#24194=CARTESIAN_POINT('',(0.,0.,0.));
#24195=CARTESIAN_POINT('',(0.,0.,0.));
#24196=CARTESIAN_POINT('Origin',(-101.730458833643,31.763829283201,198.199999999999));
#24197=CARTESIAN_POINT('',(-85.6069914720345,31.7638292832008,210.499999999999));
#24198=CARTESIAN_POINT('',(-85.6069914720345,31.7638292832008,198.199999999999));
#24199=CARTESIAN_POINT('',(-85.6069914720345,31.7638292832008,194.611133062546));
#24200=CARTESIAN_POINT('',(18.2695411663569,31.7638292831998,210.5));
#24201=CARTESIAN_POINT('',(-101.730458833643,31.763829283201,210.499999999999));
#24202=CARTESIAN_POINT('',(18.269541166357,31.7638292831998,198.2));
#24203=CARTESIAN_POINT('',(18.269541166357,31.7638292831998,198.2));
#24204=CARTESIAN_POINT('',(-101.730458833643,31.763829283201,198.199999999999));
#24205=CARTESIAN_POINT('',(17.0195411663569,31.7638292831998,208.75));
#24206=CARTESIAN_POINT('Origin',(16.2695411663569,31.7638292831998,208.75));
#24207=CARTESIAN_POINT('',(13.0195411663569,31.7638292831999,208.75));
#24208=CARTESIAN_POINT('Origin',(12.2695411663569,31.7638292831999,208.75));
#24209=CARTESIAN_POINT('',(9.0195411663569,31.7638292831999,208.75));
#24210=CARTESIAN_POINT('Origin',(8.26954116635689,31.7638292831999,208.75));
#24211=CARTESIAN_POINT('',(5.01954116635689,31.7638292831999,208.75));
#24212=CARTESIAN_POINT('Origin',(4.26954116635689,31.7638292831999,208.75));
#24213=CARTESIAN_POINT('',(1.01954116635689,31.7638292832,208.75));
#24214=CARTESIAN_POINT('Origin',(0.269541166356885,31.7638292832,208.75));
#24215=CARTESIAN_POINT('',(-2.9804588336431,31.7638292832,208.75));
#24216=CARTESIAN_POINT('Origin',(-3.7304588336431,31.7638292832,208.75));
#24217=CARTESIAN_POINT('',(-6.9804588336431,31.7638292832001,208.75));
#24218=CARTESIAN_POINT('Origin',(-7.73045883364311,31.7638292832001,208.75));
#24219=CARTESIAN_POINT('',(-10.9804588336431,31.7638292832001,208.75));
#24220=CARTESIAN_POINT('Origin',(-11.7304588336431,31.7638292832001,208.75));
#24221=CARTESIAN_POINT('',(-14.9804588336431,31.7638292832001,208.75));
#24222=CARTESIAN_POINT('Origin',(-15.7304588336431,31.7638292832001,208.75));
#24223=CARTESIAN_POINT('',(-18.9804588336431,31.7638292832002,208.75));
#24224=CARTESIAN_POINT('Origin',(-19.7304588336431,31.7638292832002,208.75));
#24225=CARTESIAN_POINT('',(-22.9804588336431,31.7638292832002,208.75));
#24226=CARTESIAN_POINT('Origin',(-23.7304588336431,31.7638292832002,208.75));
#24227=CARTESIAN_POINT('',(-26.9804588336431,31.7638292832002,208.75));
#24228=CARTESIAN_POINT('Origin',(-27.7304588336431,31.7638292832003,208.75));
#24229=CARTESIAN_POINT('',(-30.9804588336431,31.7638292832003,208.75));
#24230=CARTESIAN_POINT('Origin',(-31.7304588336431,31.7638292832003,208.75));
#24231=CARTESIAN_POINT('',(-34.9804588336431,31.7638292832003,208.75));
#24232=CARTESIAN_POINT('Origin',(-35.7304588336431,31.7638292832003,208.75));
#24233=CARTESIAN_POINT('',(-38.9804588336431,31.7638292832004,208.75));
#24234=CARTESIAN_POINT('Origin',(-39.7304588336431,31.7638292832004,208.75));
#24235=CARTESIAN_POINT('',(-42.9804588336431,31.7638292832004,208.75));
#24236=CARTESIAN_POINT('Origin',(-43.7304588336431,31.7638292832004,208.75));
#24237=CARTESIAN_POINT('',(-46.9804588336431,31.7638292832005,208.75));
#24238=CARTESIAN_POINT('Origin',(-47.7304588336431,31.7638292832005,208.75));
#24239=CARTESIAN_POINT('',(-50.9804588336431,31.7638292832005,208.749999999999));
#24240=CARTESIAN_POINT('Origin',(-51.7304588336431,31.7638292832005,208.749999999999));
#24241=CARTESIAN_POINT('',(-54.9804588336431,31.7638292832005,208.749999999999));
#24242=CARTESIAN_POINT('Origin',(-55.7304588336431,31.7638292832005,208.749999999999));
#24243=CARTESIAN_POINT('',(-58.9804588336431,31.7638292832006,208.749999999999));
#24244=CARTESIAN_POINT('Origin',(-59.7304588336431,31.7638292832006,208.749999999999));
#24245=CARTESIAN_POINT('',(-62.9804588336431,31.7638292832006,208.749999999999));
#24246=CARTESIAN_POINT('Origin',(-63.7304588336431,31.7638292832006,208.749999999999));
#24247=CARTESIAN_POINT('',(-66.9804588336431,31.7638292832006,208.749999999999));
#24248=CARTESIAN_POINT('Origin',(-67.7304588336431,31.7638292832007,208.749999999999));
#24249=CARTESIAN_POINT('',(-70.9804588336431,31.7638292832007,208.749999999999));
#24250=CARTESIAN_POINT('Origin',(-71.7304588336431,31.7638292832007,208.749999999999));
#24251=CARTESIAN_POINT('',(-74.9804588336431,31.7638292832007,208.749999999999));
#24252=CARTESIAN_POINT('Origin',(-75.7304588336431,31.7638292832007,208.749999999999));
#24253=CARTESIAN_POINT('',(-78.9804588336431,31.7638292832008,208.749999999999));
#24254=CARTESIAN_POINT('Origin',(-79.7304588336431,31.7638292832008,208.749999999999));
#24255=CARTESIAN_POINT('',(-82.9804588336431,31.7638292832008,208.749999999999));
#24256=CARTESIAN_POINT('Origin',(-83.7304588336431,31.7638292832008,208.749999999999));
#24257=CARTESIAN_POINT('',(-84.830458833643,31.7638292832008,201.549999999999));
#24258=CARTESIAN_POINT('',(-82.630458833643,31.7638292832008,201.549999999999));
#24259=CARTESIAN_POINT('',(-101.730458833643,31.763829283201,201.549999999999));
#24260=CARTESIAN_POINT('',(-82.6304588336431,31.7638292832008,204.949999999999));
#24261=CARTESIAN_POINT('',(-82.630458833643,31.7638292832008,198.199999999999));
#24262=CARTESIAN_POINT('',(-84.8304588336431,31.7638292832008,204.949999999999));
#24263=CARTESIAN_POINT('',(-101.730458833643,31.763829283201,204.949999999999));
#24264=CARTESIAN_POINT('',(-84.830458833643,31.7638292832008,198.199999999999));
#24265=CARTESIAN_POINT('',(-80.830458833643,31.7638292832008,201.549999999999));
#24266=CARTESIAN_POINT('',(-78.630458833643,31.7638292832008,201.549999999999));
#24267=CARTESIAN_POINT('',(-101.730458833643,31.763829283201,201.549999999999));
#24268=CARTESIAN_POINT('',(-78.6304588336431,31.7638292832008,204.949999999999));
#24269=CARTESIAN_POINT('',(-78.630458833643,31.7638292832008,198.199999999999));
#24270=CARTESIAN_POINT('',(-80.8304588336431,31.7638292832008,204.949999999999));
#24271=CARTESIAN_POINT('',(-101.730458833643,31.763829283201,204.949999999999));
#24272=CARTESIAN_POINT('',(-80.830458833643,31.7638292832008,198.199999999999));
#24273=CARTESIAN_POINT('',(-76.830458833643,31.7638292832008,201.549999999999));
#24274=CARTESIAN_POINT('',(-74.630458833643,31.7638292832007,201.549999999999));
#24275=CARTESIAN_POINT('',(-101.730458833643,31.763829283201,201.549999999999));
#24276=CARTESIAN_POINT('',(-74.6304588336431,31.7638292832007,204.949999999999));
#24277=CARTESIAN_POINT('',(-74.630458833643,31.7638292832007,198.199999999999));
#24278=CARTESIAN_POINT('',(-76.8304588336431,31.7638292832008,204.949999999999));
#24279=CARTESIAN_POINT('',(-101.730458833643,31.763829283201,204.949999999999));
#24280=CARTESIAN_POINT('',(-76.830458833643,31.7638292832008,198.199999999999));
#24281=CARTESIAN_POINT('',(-72.830458833643,31.7638292832007,201.549999999999));
#24282=CARTESIAN_POINT('',(-70.630458833643,31.7638292832007,201.549999999999));
#24283=CARTESIAN_POINT('',(-101.730458833643,31.763829283201,201.549999999999));
#24284=CARTESIAN_POINT('',(-70.6304588336431,31.7638292832007,204.949999999999));
#24285=CARTESIAN_POINT('',(-70.630458833643,31.7638292832007,198.199999999999));
#24286=CARTESIAN_POINT('',(-72.8304588336431,31.7638292832007,204.949999999999));
#24287=CARTESIAN_POINT('',(-101.730458833643,31.763829283201,204.949999999999));
#24288=CARTESIAN_POINT('',(-72.830458833643,31.7638292832007,198.199999999999));
#24289=CARTESIAN_POINT('',(-68.830458833643,31.7638292832007,201.549999999999));
#24290=CARTESIAN_POINT('',(-66.630458833643,31.7638292832006,201.549999999999));
#24291=CARTESIAN_POINT('',(-101.730458833643,31.763829283201,201.549999999999));
#24292=CARTESIAN_POINT('',(-66.6304588336431,31.7638292832006,204.949999999999));
#24293=CARTESIAN_POINT('',(-66.630458833643,31.7638292832006,198.199999999999));
#24294=CARTESIAN_POINT('',(-68.8304588336431,31.7638292832007,204.949999999999));
#24295=CARTESIAN_POINT('',(-101.730458833643,31.763829283201,204.949999999999));
#24296=CARTESIAN_POINT('',(-68.830458833643,31.7638292832007,198.199999999999));
#24297=CARTESIAN_POINT('',(-64.830458833643,31.7638292832006,201.549999999999));
#24298=CARTESIAN_POINT('',(-62.630458833643,31.7638292832006,201.549999999999));
#24299=CARTESIAN_POINT('',(-101.730458833643,31.763829283201,201.549999999999));
#24300=CARTESIAN_POINT('',(-62.6304588336431,31.7638292832006,204.949999999999));
#24301=CARTESIAN_POINT('',(-62.630458833643,31.7638292832006,198.199999999999));
#24302=CARTESIAN_POINT('',(-64.8304588336431,31.7638292832006,204.949999999999));
#24303=CARTESIAN_POINT('',(-101.730458833643,31.763829283201,204.949999999999));
#24304=CARTESIAN_POINT('',(-64.830458833643,31.7638292832006,198.199999999999));
#24305=CARTESIAN_POINT('',(-60.830458833643,31.7638292832006,201.549999999999));
#24306=CARTESIAN_POINT('',(-58.630458833643,31.7638292832006,201.549999999999));
#24307=CARTESIAN_POINT('',(-101.730458833643,31.763829283201,201.549999999999));
#24308=CARTESIAN_POINT('',(-58.6304588336431,31.7638292832006,204.949999999999));
#24309=CARTESIAN_POINT('',(-58.630458833643,31.7638292832006,198.199999999999));
#24310=CARTESIAN_POINT('',(-60.8304588336431,31.7638292832006,204.949999999999));
#24311=CARTESIAN_POINT('',(-101.730458833643,31.763829283201,204.949999999999));
#24312=CARTESIAN_POINT('',(-60.830458833643,31.7638292832006,198.199999999999));
#24313=CARTESIAN_POINT('',(-56.830458833643,31.7638292832006,201.549999999999));
#24314=CARTESIAN_POINT('',(-54.630458833643,31.7638292832005,201.549999999999));
#24315=CARTESIAN_POINT('',(-101.730458833643,31.763829283201,201.549999999999));
#24316=CARTESIAN_POINT('',(-54.6304588336431,31.7638292832005,204.949999999999));
#24317=CARTESIAN_POINT('',(-54.630458833643,31.7638292832005,198.199999999999));
#24318=CARTESIAN_POINT('',(-56.8304588336431,31.7638292832006,204.949999999999));
#24319=CARTESIAN_POINT('',(-101.730458833643,31.763829283201,204.949999999999));
#24320=CARTESIAN_POINT('',(-56.830458833643,31.7638292832006,198.199999999999));
#24321=CARTESIAN_POINT('',(-52.830458833643,31.7638292832005,201.549999999999));
#24322=CARTESIAN_POINT('',(-50.630458833643,31.7638292832005,201.549999999999));
#24323=CARTESIAN_POINT('',(-101.730458833643,31.763829283201,201.549999999999));
#24324=CARTESIAN_POINT('',(-50.6304588336431,31.7638292832005,204.95));
#24325=CARTESIAN_POINT('',(-50.630458833643,31.7638292832005,198.2));
#24326=CARTESIAN_POINT('',(-52.8304588336431,31.7638292832005,204.949999999999));
#24327=CARTESIAN_POINT('',(-101.730458833643,31.763829283201,204.949999999999));
#24328=CARTESIAN_POINT('',(-52.830458833643,31.7638292832005,198.2));
#24329=CARTESIAN_POINT('',(-48.830458833643,31.7638292832005,201.549999999999));
#24330=CARTESIAN_POINT('',(-46.630458833643,31.7638292832005,201.55));
#24331=CARTESIAN_POINT('',(-101.730458833643,31.763829283201,201.549999999999));
#24332=CARTESIAN_POINT('',(-46.6304588336431,31.7638292832005,204.95));
#24333=CARTESIAN_POINT('',(-46.630458833643,31.7638292832005,198.2));
#24334=CARTESIAN_POINT('',(-48.8304588336431,31.7638292832005,204.95));
#24335=CARTESIAN_POINT('',(-101.730458833643,31.763829283201,204.949999999999));
#24336=CARTESIAN_POINT('',(-48.830458833643,31.7638292832005,198.2));
#24337=CARTESIAN_POINT('',(-44.830458833643,31.7638292832004,201.55));
#24338=CARTESIAN_POINT('',(-42.630458833643,31.7638292832004,201.55));
#24339=CARTESIAN_POINT('',(-101.730458833643,31.763829283201,201.549999999999));
#24340=CARTESIAN_POINT('',(-42.6304588336431,31.7638292832004,204.95));
#24341=CARTESIAN_POINT('',(-42.630458833643,31.7638292832004,198.2));
#24342=CARTESIAN_POINT('',(-44.8304588336431,31.7638292832004,204.95));
#24343=CARTESIAN_POINT('',(-101.730458833643,31.763829283201,204.949999999999));
#24344=CARTESIAN_POINT('',(-44.830458833643,31.7638292832004,198.2));
#24345=CARTESIAN_POINT('',(-40.830458833643,31.7638292832004,201.55));
#24346=CARTESIAN_POINT('',(-38.630458833643,31.7638292832004,201.55));
#24347=CARTESIAN_POINT('',(-101.730458833643,31.763829283201,201.549999999999));
#24348=CARTESIAN_POINT('',(-38.6304588336431,31.7638292832004,204.95));
#24349=CARTESIAN_POINT('',(-38.630458833643,31.7638292832004,198.2));
#24350=CARTESIAN_POINT('',(-40.8304588336431,31.7638292832004,204.95));
#24351=CARTESIAN_POINT('',(-101.730458833643,31.763829283201,204.949999999999));
#24352=CARTESIAN_POINT('',(-40.830458833643,31.7638292832004,198.2));
#24353=CARTESIAN_POINT('',(-36.830458833643,31.7638292832003,201.55));
#24354=CARTESIAN_POINT('',(-34.630458833643,31.7638292832003,201.55));
#24355=CARTESIAN_POINT('',(-101.730458833643,31.763829283201,201.549999999999));
#24356=CARTESIAN_POINT('',(-34.6304588336431,31.7638292832003,204.95));
#24357=CARTESIAN_POINT('',(-34.630458833643,31.7638292832003,198.2));
#24358=CARTESIAN_POINT('',(-36.8304588336431,31.7638292832003,204.95));
#24359=CARTESIAN_POINT('',(-101.730458833643,31.763829283201,204.949999999999));
#24360=CARTESIAN_POINT('',(-36.830458833643,31.7638292832003,198.2));
#24361=CARTESIAN_POINT('',(-32.830458833643,31.7638292832003,201.55));
#24362=CARTESIAN_POINT('',(-30.630458833643,31.7638292832003,201.55));
#24363=CARTESIAN_POINT('',(-101.730458833643,31.763829283201,201.549999999999));
#24364=CARTESIAN_POINT('',(-30.6304588336431,31.7638292832003,204.95));
#24365=CARTESIAN_POINT('',(-30.630458833643,31.7638292832003,198.2));
#24366=CARTESIAN_POINT('',(-32.8304588336431,31.7638292832003,204.95));
#24367=CARTESIAN_POINT('',(-101.730458833643,31.763829283201,204.949999999999));
#24368=CARTESIAN_POINT('',(-32.830458833643,31.7638292832003,198.2));
#24369=CARTESIAN_POINT('',(-28.830458833643,31.7638292832003,201.55));
#24370=CARTESIAN_POINT('',(-26.630458833643,31.7638292832003,201.55));
#24371=CARTESIAN_POINT('',(-101.730458833643,31.763829283201,201.549999999999));
#24372=CARTESIAN_POINT('',(-26.6304588336431,31.7638292832003,204.95));
#24373=CARTESIAN_POINT('',(-26.630458833643,31.7638292832003,198.2));
#24374=CARTESIAN_POINT('',(-28.8304588336431,31.7638292832003,204.95));
#24375=CARTESIAN_POINT('',(-101.730458833643,31.763829283201,204.949999999999));
#24376=CARTESIAN_POINT('',(-28.830458833643,31.7638292832003,198.2));
#24377=CARTESIAN_POINT('',(-24.830458833643,31.7638292832002,201.55));
#24378=CARTESIAN_POINT('',(-22.630458833643,31.7638292832002,201.55));
#24379=CARTESIAN_POINT('',(-101.730458833643,31.763829283201,201.549999999999));
#24380=CARTESIAN_POINT('',(-22.6304588336431,31.7638292832002,204.95));
#24381=CARTESIAN_POINT('',(-22.630458833643,31.7638292832002,198.2));
#24382=CARTESIAN_POINT('',(-24.8304588336431,31.7638292832002,204.95));
#24383=CARTESIAN_POINT('',(-101.730458833643,31.763829283201,204.949999999999));
#24384=CARTESIAN_POINT('',(-24.830458833643,31.7638292832002,198.2));
#24385=CARTESIAN_POINT('',(-20.830458833643,31.7638292832002,201.55));
#24386=CARTESIAN_POINT('',(-18.630458833643,31.7638292832002,201.55));
#24387=CARTESIAN_POINT('',(-101.730458833643,31.763829283201,201.549999999999));
#24388=CARTESIAN_POINT('',(-18.6304588336431,31.7638292832002,204.95));
#24389=CARTESIAN_POINT('',(-18.630458833643,31.7638292832002,198.2));
#24390=CARTESIAN_POINT('',(-20.8304588336431,31.7638292832002,204.95));
#24391=CARTESIAN_POINT('',(-101.730458833643,31.763829283201,204.949999999999));
#24392=CARTESIAN_POINT('',(-20.830458833643,31.7638292832002,198.2));
#24393=CARTESIAN_POINT('',(-16.830458833643,31.7638292832002,201.55));
#24394=CARTESIAN_POINT('',(-14.630458833643,31.7638292832001,201.55));
#24395=CARTESIAN_POINT('',(-101.730458833643,31.763829283201,201.549999999999));
#24396=CARTESIAN_POINT('',(-14.6304588336431,31.7638292832001,204.95));
#24397=CARTESIAN_POINT('',(-14.630458833643,31.7638292832001,198.2));
#24398=CARTESIAN_POINT('',(-16.8304588336431,31.7638292832002,204.95));
#24399=CARTESIAN_POINT('',(-101.730458833643,31.763829283201,204.949999999999));
#24400=CARTESIAN_POINT('',(-16.830458833643,31.7638292832002,198.2));
#24401=CARTESIAN_POINT('',(-12.830458833643,31.7638292832001,201.55));
#24402=CARTESIAN_POINT('',(-10.630458833643,31.7638292832001,201.55));
#24403=CARTESIAN_POINT('',(-101.730458833643,31.763829283201,201.549999999999));
#24404=CARTESIAN_POINT('',(-10.6304588336431,31.7638292832001,204.95));
#24405=CARTESIAN_POINT('',(-10.630458833643,31.7638292832001,198.2));
#24406=CARTESIAN_POINT('',(-12.8304588336431,31.7638292832001,204.95));
#24407=CARTESIAN_POINT('',(-101.730458833643,31.763829283201,204.949999999999));
#24408=CARTESIAN_POINT('',(-12.830458833643,31.7638292832001,198.2));
#24409=CARTESIAN_POINT('',(-8.83045883364303,31.7638292832001,201.55));
#24410=CARTESIAN_POINT('',(-6.63045883364302,31.7638292832,201.55));
#24411=CARTESIAN_POINT('',(-101.730458833643,31.763829283201,201.549999999999));
#24412=CARTESIAN_POINT('',(-6.63045883364306,31.7638292832,204.95));
#24413=CARTESIAN_POINT('',(-6.63045883364299,31.7638292832,198.2));
#24414=CARTESIAN_POINT('',(-8.83045883364307,31.7638292832001,204.95));
#24415=CARTESIAN_POINT('',(-101.730458833643,31.763829283201,204.949999999999));
#24416=CARTESIAN_POINT('',(-8.830458833643,31.7638292832001,198.2));
#24417=CARTESIAN_POINT('',(-4.83045883364302,31.7638292832,201.55));
#24418=CARTESIAN_POINT('',(-2.63045883364303,31.7638292832,201.55));
#24419=CARTESIAN_POINT('',(-101.730458833643,31.763829283201,201.549999999999));
#24420=CARTESIAN_POINT('',(-2.63045883364307,31.7638292832,204.95));
#24421=CARTESIAN_POINT('',(-2.630458833643,31.7638292832,198.2));
#24422=CARTESIAN_POINT('',(-4.83045883364307,31.7638292832,204.95));
#24423=CARTESIAN_POINT('',(-101.730458833643,31.763829283201,204.949999999999));
#24424=CARTESIAN_POINT('',(-4.830458833643,31.7638292832,198.2));
#24425=CARTESIAN_POINT('',(-0.830458833643022,31.7638292832,201.55));
#24426=CARTESIAN_POINT('',(1.36954116635697,31.7638292832,201.55));
#24427=CARTESIAN_POINT('',(-101.730458833643,31.763829283201,201.549999999999));
#24428=CARTESIAN_POINT('',(1.36954116635693,31.7638292832,204.95));
#24429=CARTESIAN_POINT('',(1.369541166357,31.7638292832,198.2));
#24430=CARTESIAN_POINT('',(-0.830458833643063,31.7638292832,204.95));
#24431=CARTESIAN_POINT('',(-101.730458833643,31.763829283201,204.949999999999));
#24432=CARTESIAN_POINT('',(-0.830458833642994,31.7638292832,198.2));
#24433=CARTESIAN_POINT('',(3.16954116635697,31.7638292832,201.55));
#24434=CARTESIAN_POINT('',(5.36954116635698,31.7638292831999,201.55));
#24435=CARTESIAN_POINT('',(-101.730458833643,31.763829283201,201.549999999999));
#24436=CARTESIAN_POINT('',(5.36954116635693,31.7638292831999,204.95));
#24437=CARTESIAN_POINT('',(5.369541166357,31.7638292831999,198.2));
#24438=CARTESIAN_POINT('',(3.16954116635693,31.7638292832,204.95));
#24439=CARTESIAN_POINT('',(-101.730458833643,31.763829283201,204.949999999999));
#24440=CARTESIAN_POINT('',(3.169541166357,31.7638292832,198.2));
#24441=CARTESIAN_POINT('',(7.16954116635697,31.7638292831999,201.55));
#24442=CARTESIAN_POINT('',(9.36954116635698,31.7638292831999,201.55));
#24443=CARTESIAN_POINT('',(-101.730458833643,31.763829283201,201.549999999999));
#24444=CARTESIAN_POINT('',(9.36954116635694,31.7638292831999,204.95));
#24445=CARTESIAN_POINT('',(9.36954116635701,31.7638292831999,198.2));
#24446=CARTESIAN_POINT('',(7.16954116635693,31.7638292831999,204.95));
#24447=CARTESIAN_POINT('',(-101.730458833643,31.763829283201,204.949999999999));
#24448=CARTESIAN_POINT('',(7.169541166357,31.7638292831999,198.2));
#24449=CARTESIAN_POINT('',(11.169541166357,31.7638292831999,201.55));
#24450=CARTESIAN_POINT('',(13.369541166357,31.7638292831998,201.55));
#24451=CARTESIAN_POINT('',(-101.730458833643,31.763829283201,201.549999999999));
#24452=CARTESIAN_POINT('',(13.3695411663569,31.7638292831998,204.95));
#24453=CARTESIAN_POINT('',(13.369541166357,31.7638292831998,198.2));
#24454=CARTESIAN_POINT('',(11.1695411663569,31.7638292831999,204.95));
#24455=CARTESIAN_POINT('',(-101.730458833643,31.763829283201,204.949999999999));
#24456=CARTESIAN_POINT('',(11.169541166357,31.7638292831999,198.2));
#24457=CARTESIAN_POINT('',(15.169541166357,31.7638292831998,201.55));
#24458=CARTESIAN_POINT('',(17.369541166357,31.7638292831998,201.55));
#24459=CARTESIAN_POINT('',(-101.730458833643,31.763829283201,201.549999999999));
#24460=CARTESIAN_POINT('',(17.3695411663569,31.7638292831998,204.95));
#24461=CARTESIAN_POINT('',(17.369541166357,31.7638292831998,198.2));
#24462=CARTESIAN_POINT('',(15.1695411663569,31.7638292831998,204.95));
#24463=CARTESIAN_POINT('',(-101.730458833643,31.763829283201,204.949999999999));
#24464=CARTESIAN_POINT('',(15.169541166357,31.7638292831998,198.2));
#24465=CARTESIAN_POINT('Origin',(-101.730458833643,31.263829283201,198.199999999999));
#24466=CARTESIAN_POINT('',(-85.6069914720345,31.2638292831998,198.199999999999));
#24467=CARTESIAN_POINT('',(-85.6069914720345,31.2638292832008,210.5));
#24468=CARTESIAN_POINT('',(-85.6069914720345,31.2638292832008,198.199999999999));
#24469=CARTESIAN_POINT('',(18.269541166357,31.2638292831998,198.2));
#24470=CARTESIAN_POINT('',(-101.730458833643,31.263829283201,198.199999999999));
#24471=CARTESIAN_POINT('',(18.2695411663569,31.2638292831998,210.5));
#24472=CARTESIAN_POINT('',(18.269541166357,31.2638292831998,198.2));
#24473=CARTESIAN_POINT('',(-101.730458833643,31.263829283201,210.499999999999));
#24474=CARTESIAN_POINT('',(15.169541166357,31.2638292831998,201.55));
#24475=CARTESIAN_POINT('',(17.369541166357,31.2638292831998,201.55));
#24476=CARTESIAN_POINT('',(-101.730458833643,31.263829283201,201.549999999999));
#24477=CARTESIAN_POINT('',(15.1695411663569,31.2638292831998,204.95));
#24478=CARTESIAN_POINT('',(15.169541166357,31.2638292831998,198.2));
#24479=CARTESIAN_POINT('',(17.3695411663569,31.2638292831998,204.95));
#24480=CARTESIAN_POINT('',(-101.730458833643,31.263829283201,204.949999999999));
#24481=CARTESIAN_POINT('',(17.369541166357,31.2638292831998,198.2));
#24482=CARTESIAN_POINT('',(11.169541166357,31.2638292831999,201.55));
#24483=CARTESIAN_POINT('',(13.369541166357,31.2638292831998,201.55));
#24484=CARTESIAN_POINT('',(-101.730458833643,31.263829283201,201.549999999999));
#24485=CARTESIAN_POINT('',(11.1695411663569,31.2638292831999,204.95));
#24486=CARTESIAN_POINT('',(11.169541166357,31.2638292831999,198.2));
#24487=CARTESIAN_POINT('',(13.3695411663569,31.2638292831998,204.95));
#24488=CARTESIAN_POINT('',(-101.730458833643,31.263829283201,204.949999999999));
#24489=CARTESIAN_POINT('',(13.369541166357,31.2638292831998,198.2));
#24490=CARTESIAN_POINT('',(7.16954116635697,31.2638292831999,201.55));
#24491=CARTESIAN_POINT('',(9.36954116635698,31.2638292831999,201.55));
#24492=CARTESIAN_POINT('',(-101.730458833643,31.263829283201,201.549999999999));
#24493=CARTESIAN_POINT('',(7.16954116635693,31.2638292831999,204.95));
#24494=CARTESIAN_POINT('',(7.169541166357,31.2638292831999,198.2));
#24495=CARTESIAN_POINT('',(9.36954116635694,31.2638292831999,204.95));
#24496=CARTESIAN_POINT('',(-101.730458833643,31.263829283201,204.949999999999));
#24497=CARTESIAN_POINT('',(9.36954116635701,31.2638292831999,198.2));
#24498=CARTESIAN_POINT('',(3.16954116635697,31.2638292832,201.55));
#24499=CARTESIAN_POINT('',(5.36954116635698,31.2638292831999,201.55));
#24500=CARTESIAN_POINT('',(-101.730458833643,31.263829283201,201.549999999999));
#24501=CARTESIAN_POINT('',(3.16954116635693,31.2638292832,204.95));
#24502=CARTESIAN_POINT('',(3.169541166357,31.2638292832,198.2));
#24503=CARTESIAN_POINT('',(5.36954116635693,31.2638292831999,204.95));
#24504=CARTESIAN_POINT('',(-101.730458833643,31.263829283201,204.949999999999));
#24505=CARTESIAN_POINT('',(5.369541166357,31.2638292831999,198.2));
#24506=CARTESIAN_POINT('',(-0.830458833643022,31.2638292832,201.55));
#24507=CARTESIAN_POINT('',(1.36954116635697,31.2638292832,201.55));
#24508=CARTESIAN_POINT('',(-101.730458833643,31.263829283201,201.549999999999));
#24509=CARTESIAN_POINT('',(-0.830458833643063,31.2638292832,204.95));
#24510=CARTESIAN_POINT('',(-0.830458833642994,31.2638292832,198.2));
#24511=CARTESIAN_POINT('',(1.36954116635693,31.2638292832,204.95));
#24512=CARTESIAN_POINT('',(-101.730458833643,31.263829283201,204.949999999999));
#24513=CARTESIAN_POINT('',(1.369541166357,31.2638292832,198.2));
#24514=CARTESIAN_POINT('',(-4.83045883364302,31.2638292832,201.55));
#24515=CARTESIAN_POINT('',(-2.63045883364303,31.2638292832,201.55));
#24516=CARTESIAN_POINT('',(-101.730458833643,31.263829283201,201.549999999999));
#24517=CARTESIAN_POINT('',(-4.83045883364307,31.2638292832,204.95));
#24518=CARTESIAN_POINT('',(-4.830458833643,31.2638292832,198.2));
#24519=CARTESIAN_POINT('',(-2.63045883364307,31.2638292832,204.95));
#24520=CARTESIAN_POINT('',(-101.730458833643,31.263829283201,204.949999999999));
#24521=CARTESIAN_POINT('',(-2.630458833643,31.2638292832,198.2));
#24522=CARTESIAN_POINT('',(-8.83045883364303,31.2638292832001,201.55));
#24523=CARTESIAN_POINT('',(-6.63045883364302,31.2638292832,201.55));
#24524=CARTESIAN_POINT('',(-101.730458833643,31.263829283201,201.549999999999));
#24525=CARTESIAN_POINT('',(-8.83045883364307,31.2638292832001,204.95));
#24526=CARTESIAN_POINT('',(-8.830458833643,31.2638292832001,198.2));
#24527=CARTESIAN_POINT('',(-6.63045883364306,31.2638292832,204.95));
#24528=CARTESIAN_POINT('',(-101.730458833643,31.263829283201,204.949999999999));
#24529=CARTESIAN_POINT('',(-6.63045883364299,31.2638292832,198.2));
#24530=CARTESIAN_POINT('',(-12.830458833643,31.2638292832001,201.55));
#24531=CARTESIAN_POINT('',(-10.630458833643,31.2638292832001,201.55));
#24532=CARTESIAN_POINT('',(-101.730458833643,31.263829283201,201.549999999999));
#24533=CARTESIAN_POINT('',(-12.8304588336431,31.2638292832001,204.95));
#24534=CARTESIAN_POINT('',(-12.830458833643,31.2638292832001,198.2));
#24535=CARTESIAN_POINT('',(-10.6304588336431,31.2638292832001,204.95));
#24536=CARTESIAN_POINT('',(-101.730458833643,31.263829283201,204.949999999999));
#24537=CARTESIAN_POINT('',(-10.630458833643,31.2638292832001,198.2));
#24538=CARTESIAN_POINT('',(-16.830458833643,31.2638292832002,201.55));
#24539=CARTESIAN_POINT('',(-14.630458833643,31.2638292832001,201.55));
#24540=CARTESIAN_POINT('',(-101.730458833643,31.263829283201,201.549999999999));
#24541=CARTESIAN_POINT('',(-16.8304588336431,31.2638292832002,204.95));
#24542=CARTESIAN_POINT('',(-16.830458833643,31.2638292832002,198.2));
#24543=CARTESIAN_POINT('',(-14.6304588336431,31.2638292832001,204.95));
#24544=CARTESIAN_POINT('',(-101.730458833643,31.263829283201,204.949999999999));
#24545=CARTESIAN_POINT('',(-14.630458833643,31.2638292832001,198.2));
#24546=CARTESIAN_POINT('',(-20.830458833643,31.2638292832002,201.55));
#24547=CARTESIAN_POINT('',(-18.630458833643,31.2638292832002,201.55));
#24548=CARTESIAN_POINT('',(-101.730458833643,31.263829283201,201.549999999999));
#24549=CARTESIAN_POINT('',(-20.8304588336431,31.2638292832002,204.95));
#24550=CARTESIAN_POINT('',(-20.830458833643,31.2638292832002,198.2));
#24551=CARTESIAN_POINT('',(-18.6304588336431,31.2638292832002,204.95));
#24552=CARTESIAN_POINT('',(-101.730458833643,31.263829283201,204.949999999999));
#24553=CARTESIAN_POINT('',(-18.630458833643,31.2638292832002,198.2));
#24554=CARTESIAN_POINT('',(-24.830458833643,31.2638292832002,201.55));
#24555=CARTESIAN_POINT('',(-22.630458833643,31.2638292832002,201.55));
#24556=CARTESIAN_POINT('',(-101.730458833643,31.263829283201,201.549999999999));
#24557=CARTESIAN_POINT('',(-24.8304588336431,31.2638292832002,204.95));
#24558=CARTESIAN_POINT('',(-24.830458833643,31.2638292832002,198.2));
#24559=CARTESIAN_POINT('',(-22.6304588336431,31.2638292832002,204.95));
#24560=CARTESIAN_POINT('',(-101.730458833643,31.263829283201,204.949999999999));
#24561=CARTESIAN_POINT('',(-22.630458833643,31.2638292832002,198.2));
#24562=CARTESIAN_POINT('',(-28.830458833643,31.2638292832003,201.55));
#24563=CARTESIAN_POINT('',(-26.630458833643,31.2638292832002,201.55));
#24564=CARTESIAN_POINT('',(-101.730458833643,31.263829283201,201.549999999999));
#24565=CARTESIAN_POINT('',(-28.8304588336431,31.2638292832003,204.95));
#24566=CARTESIAN_POINT('',(-28.830458833643,31.2638292832003,198.2));
#24567=CARTESIAN_POINT('',(-26.6304588336431,31.2638292832002,204.95));
#24568=CARTESIAN_POINT('',(-101.730458833643,31.263829283201,204.949999999999));
#24569=CARTESIAN_POINT('',(-26.630458833643,31.2638292832002,198.2));
#24570=CARTESIAN_POINT('',(-32.830458833643,31.2638292832003,201.55));
#24571=CARTESIAN_POINT('',(-30.630458833643,31.2638292832003,201.55));
#24572=CARTESIAN_POINT('',(-101.730458833643,31.263829283201,201.549999999999));
#24573=CARTESIAN_POINT('',(-32.8304588336431,31.2638292832003,204.95));
#24574=CARTESIAN_POINT('',(-32.830458833643,31.2638292832003,198.2));
#24575=CARTESIAN_POINT('',(-30.6304588336431,31.2638292832003,204.95));
#24576=CARTESIAN_POINT('',(-101.730458833643,31.263829283201,204.949999999999));
#24577=CARTESIAN_POINT('',(-30.630458833643,31.2638292832003,198.2));
#24578=CARTESIAN_POINT('',(-36.830458833643,31.2638292832004,201.55));
#24579=CARTESIAN_POINT('',(-34.630458833643,31.2638292832003,201.55));
#24580=CARTESIAN_POINT('',(-101.730458833643,31.263829283201,201.549999999999));
#24581=CARTESIAN_POINT('',(-36.8304588336431,31.2638292832004,204.95));
#24582=CARTESIAN_POINT('',(-36.830458833643,31.2638292832004,198.2));
#24583=CARTESIAN_POINT('',(-34.6304588336431,31.2638292832003,204.95));
#24584=CARTESIAN_POINT('',(-101.730458833643,31.263829283201,204.949999999999));
#24585=CARTESIAN_POINT('',(-34.630458833643,31.2638292832003,198.2));
#24586=CARTESIAN_POINT('',(-40.830458833643,31.2638292832004,201.55));
#24587=CARTESIAN_POINT('',(-38.630458833643,31.2638292832004,201.55));
#24588=CARTESIAN_POINT('',(-101.730458833643,31.263829283201,201.549999999999));
#24589=CARTESIAN_POINT('',(-40.8304588336431,31.2638292832004,204.95));
#24590=CARTESIAN_POINT('',(-40.830458833643,31.2638292832004,198.2));
#24591=CARTESIAN_POINT('',(-38.6304588336431,31.2638292832004,204.95));
#24592=CARTESIAN_POINT('',(-101.730458833643,31.263829283201,204.949999999999));
#24593=CARTESIAN_POINT('',(-38.630458833643,31.2638292832004,198.2));
#24594=CARTESIAN_POINT('',(-44.830458833643,31.2638292832004,201.55));
#24595=CARTESIAN_POINT('',(-42.630458833643,31.2638292832004,201.55));
#24596=CARTESIAN_POINT('',(-101.730458833643,31.263829283201,201.549999999999));
#24597=CARTESIAN_POINT('',(-44.8304588336431,31.2638292832004,204.95));
#24598=CARTESIAN_POINT('',(-44.830458833643,31.2638292832004,198.2));
#24599=CARTESIAN_POINT('',(-42.6304588336431,31.2638292832004,204.95));
#24600=CARTESIAN_POINT('',(-101.730458833643,31.263829283201,204.949999999999));
#24601=CARTESIAN_POINT('',(-42.630458833643,31.2638292832004,198.2));
#24602=CARTESIAN_POINT('',(-48.830458833643,31.2638292832005,201.549999999999));
#24603=CARTESIAN_POINT('',(-46.630458833643,31.2638292832004,201.55));
#24604=CARTESIAN_POINT('',(-101.730458833643,31.263829283201,201.549999999999));
#24605=CARTESIAN_POINT('',(-48.8304588336431,31.2638292832005,204.95));
#24606=CARTESIAN_POINT('',(-48.830458833643,31.2638292832005,198.2));
#24607=CARTESIAN_POINT('',(-46.6304588336431,31.2638292832004,204.95));
#24608=CARTESIAN_POINT('',(-101.730458833643,31.263829283201,204.949999999999));
#24609=CARTESIAN_POINT('',(-46.630458833643,31.2638292832004,198.2));
#24610=CARTESIAN_POINT('',(-52.830458833643,31.2638292832005,201.549999999999));
#24611=CARTESIAN_POINT('',(-50.630458833643,31.2638292832005,201.549999999999));
#24612=CARTESIAN_POINT('',(-101.730458833643,31.263829283201,201.549999999999));
#24613=CARTESIAN_POINT('',(-52.8304588336431,31.2638292832005,204.949999999999));
#24614=CARTESIAN_POINT('',(-52.830458833643,31.2638292832005,198.2));
#24615=CARTESIAN_POINT('',(-50.6304588336431,31.2638292832005,204.95));
#24616=CARTESIAN_POINT('',(-101.730458833643,31.263829283201,204.949999999999));
#24617=CARTESIAN_POINT('',(-50.630458833643,31.2638292832005,198.2));
#24618=CARTESIAN_POINT('',(-56.830458833643,31.2638292832006,201.549999999999));
#24619=CARTESIAN_POINT('',(-54.630458833643,31.2638292832005,201.549999999999));
#24620=CARTESIAN_POINT('',(-101.730458833643,31.263829283201,201.549999999999));
#24621=CARTESIAN_POINT('',(-56.8304588336431,31.2638292832006,204.949999999999));
#24622=CARTESIAN_POINT('',(-56.830458833643,31.2638292832006,198.199999999999));
#24623=CARTESIAN_POINT('',(-54.6304588336431,31.2638292832005,204.949999999999));
#24624=CARTESIAN_POINT('',(-101.730458833643,31.263829283201,204.949999999999));
#24625=CARTESIAN_POINT('',(-54.630458833643,31.2638292832005,198.199999999999));
#24626=CARTESIAN_POINT('',(-60.830458833643,31.2638292832006,201.549999999999));
#24627=CARTESIAN_POINT('',(-58.630458833643,31.2638292832006,201.549999999999));
#24628=CARTESIAN_POINT('',(-101.730458833643,31.263829283201,201.549999999999));
#24629=CARTESIAN_POINT('',(-60.8304588336431,31.2638292832006,204.949999999999));
#24630=CARTESIAN_POINT('',(-60.830458833643,31.2638292832006,198.199999999999));
#24631=CARTESIAN_POINT('',(-58.6304588336431,31.2638292832006,204.949999999999));
#24632=CARTESIAN_POINT('',(-101.730458833643,31.263829283201,204.949999999999));
#24633=CARTESIAN_POINT('',(-58.630458833643,31.2638292832006,198.199999999999));
#24634=CARTESIAN_POINT('',(-64.830458833643,31.2638292832006,201.549999999999));
#24635=CARTESIAN_POINT('',(-62.6304588336431,31.2638292832006,201.549999999999));
#24636=CARTESIAN_POINT('',(-101.730458833643,31.263829283201,201.549999999999));
#24637=CARTESIAN_POINT('',(-64.8304588336431,31.2638292832006,204.949999999999));
#24638=CARTESIAN_POINT('',(-64.830458833643,31.2638292832006,198.199999999999));
#24639=CARTESIAN_POINT('',(-62.6304588336431,31.2638292832006,204.949999999999));
#24640=CARTESIAN_POINT('',(-101.730458833643,31.263829283201,204.949999999999));
#24641=CARTESIAN_POINT('',(-62.630458833643,31.2638292832006,198.199999999999));
#24642=CARTESIAN_POINT('',(-68.830458833643,31.2638292832007,201.549999999999));
#24643=CARTESIAN_POINT('',(-66.630458833643,31.2638292832006,201.549999999999));
#24644=CARTESIAN_POINT('',(-101.730458833643,31.263829283201,201.549999999999));
#24645=CARTESIAN_POINT('',(-68.8304588336431,31.2638292832007,204.949999999999));
#24646=CARTESIAN_POINT('',(-68.830458833643,31.2638292832007,198.199999999999));
#24647=CARTESIAN_POINT('',(-66.6304588336431,31.2638292832006,204.949999999999));
#24648=CARTESIAN_POINT('',(-101.730458833643,31.263829283201,204.949999999999));
#24649=CARTESIAN_POINT('',(-66.630458833643,31.2638292832006,198.199999999999));
#24650=CARTESIAN_POINT('',(-72.830458833643,31.2638292832007,201.549999999999));
#24651=CARTESIAN_POINT('',(-70.630458833643,31.2638292832007,201.549999999999));
#24652=CARTESIAN_POINT('',(-101.730458833643,31.263829283201,201.549999999999));
#24653=CARTESIAN_POINT('',(-72.8304588336431,31.2638292832007,204.949999999999));
#24654=CARTESIAN_POINT('',(-72.830458833643,31.2638292832007,198.199999999999));
#24655=CARTESIAN_POINT('',(-70.6304588336431,31.2638292832007,204.949999999999));
#24656=CARTESIAN_POINT('',(-101.730458833643,31.263829283201,204.949999999999));
#24657=CARTESIAN_POINT('',(-70.630458833643,31.2638292832007,198.199999999999));
#24658=CARTESIAN_POINT('',(-76.830458833643,31.2638292832007,201.549999999999));
#24659=CARTESIAN_POINT('',(-74.630458833643,31.2638292832007,201.549999999999));
#24660=CARTESIAN_POINT('',(-101.730458833643,31.263829283201,201.549999999999));
#24661=CARTESIAN_POINT('',(-76.8304588336431,31.2638292832007,204.949999999999));
#24662=CARTESIAN_POINT('',(-76.830458833643,31.2638292832007,198.199999999999));
#24663=CARTESIAN_POINT('',(-74.6304588336431,31.2638292832007,204.949999999999));
#24664=CARTESIAN_POINT('',(-101.730458833643,31.263829283201,204.949999999999));
#24665=CARTESIAN_POINT('',(-74.630458833643,31.2638292832007,198.199999999999));
#24666=CARTESIAN_POINT('',(-80.830458833643,31.2638292832008,201.549999999999));
#24667=CARTESIAN_POINT('',(-78.630458833643,31.2638292832008,201.549999999999));
#24668=CARTESIAN_POINT('',(-101.730458833643,31.263829283201,201.549999999999));
#24669=CARTESIAN_POINT('',(-80.8304588336431,31.2638292832008,204.949999999999));
#24670=CARTESIAN_POINT('',(-80.830458833643,31.2638292832008,198.199999999999));
#24671=CARTESIAN_POINT('',(-78.6304588336431,31.2638292832008,204.949999999999));
#24672=CARTESIAN_POINT('',(-101.730458833643,31.263829283201,204.949999999999));
#24673=CARTESIAN_POINT('',(-78.630458833643,31.2638292832008,198.199999999999));
#24674=CARTESIAN_POINT('',(-84.830458833643,31.2638292832008,201.549999999999));
#24675=CARTESIAN_POINT('',(-82.630458833643,31.2638292832008,201.549999999999));
#24676=CARTESIAN_POINT('',(-101.730458833643,31.263829283201,201.549999999999));
#24677=CARTESIAN_POINT('',(-84.8304588336431,31.2638292832008,204.949999999999));
#24678=CARTESIAN_POINT('',(-84.830458833643,31.2638292832008,198.199999999999));
#24679=CARTESIAN_POINT('',(-82.6304588336431,31.2638292832008,204.949999999999));
#24680=CARTESIAN_POINT('',(-101.730458833643,31.263829283201,204.949999999999));
#24681=CARTESIAN_POINT('',(-82.630458833643,31.2638292832008,198.199999999999));
#24682=CARTESIAN_POINT('',(-82.9804588336431,31.2638292832008,208.749999999999));
#24683=CARTESIAN_POINT('Origin',(-83.7304588336431,31.2638292832008,208.749999999999));
#24684=CARTESIAN_POINT('',(-78.9804588336431,31.2638292832008,208.749999999999));
#24685=CARTESIAN_POINT('Origin',(-79.7304588336431,31.2638292832008,208.749999999999));
#24686=CARTESIAN_POINT('',(-74.9804588336431,31.2638292832007,208.749999999999));
#24687=CARTESIAN_POINT('Origin',(-75.7304588336431,31.2638292832007,208.749999999999));
#24688=CARTESIAN_POINT('',(-70.9804588336431,31.2638292832007,208.749999999999));
#24689=CARTESIAN_POINT('Origin',(-71.7304588336431,31.2638292832007,208.749999999999));
#24690=CARTESIAN_POINT('',(-66.9804588336431,31.2638292832006,208.749999999999));
#24691=CARTESIAN_POINT('Origin',(-67.7304588336431,31.2638292832007,208.749999999999));
#24692=CARTESIAN_POINT('',(-62.9804588336431,31.2638292832006,208.749999999999));
#24693=CARTESIAN_POINT('Origin',(-63.7304588336431,31.2638292832006,208.749999999999));
#24694=CARTESIAN_POINT('',(-58.9804588336431,31.2638292832006,208.749999999999));
#24695=CARTESIAN_POINT('Origin',(-59.7304588336431,31.2638292832006,208.749999999999));
#24696=CARTESIAN_POINT('',(-54.9804588336431,31.2638292832005,208.749999999999));
#24697=CARTESIAN_POINT('Origin',(-55.7304588336431,31.2638292832005,208.749999999999));
#24698=CARTESIAN_POINT('',(-50.9804588336431,31.2638292832005,208.749999999999));
#24699=CARTESIAN_POINT('Origin',(-51.7304588336431,31.2638292832005,208.749999999999));
#24700=CARTESIAN_POINT('',(-46.9804588336431,31.2638292832004,208.75));
#24701=CARTESIAN_POINT('Origin',(-47.7304588336431,31.2638292832005,208.75));
#24702=CARTESIAN_POINT('',(-42.9804588336431,31.2638292832004,208.75));
#24703=CARTESIAN_POINT('Origin',(-43.7304588336431,31.2638292832004,208.75));
#24704=CARTESIAN_POINT('',(-38.9804588336431,31.2638292832004,208.75));
#24705=CARTESIAN_POINT('Origin',(-39.7304588336431,31.2638292832004,208.75));
#24706=CARTESIAN_POINT('',(-34.9804588336431,31.2638292832003,208.75));
#24707=CARTESIAN_POINT('Origin',(-35.7304588336431,31.2638292832003,208.75));
#24708=CARTESIAN_POINT('',(-30.9804588336431,31.2638292832003,208.75));
#24709=CARTESIAN_POINT('Origin',(-31.7304588336431,31.2638292832003,208.75));
#24710=CARTESIAN_POINT('',(-26.9804588336431,31.2638292832002,208.75));
#24711=CARTESIAN_POINT('Origin',(-27.7304588336431,31.2638292832003,208.75));
#24712=CARTESIAN_POINT('',(-22.9804588336431,31.2638292832002,208.75));
#24713=CARTESIAN_POINT('Origin',(-23.7304588336431,31.2638292832002,208.75));
#24714=CARTESIAN_POINT('',(-18.9804588336431,31.2638292832002,208.75));
#24715=CARTESIAN_POINT('Origin',(-19.7304588336431,31.2638292832002,208.75));
#24716=CARTESIAN_POINT('',(-14.9804588336431,31.2638292832001,208.75));
#24717=CARTESIAN_POINT('Origin',(-15.7304588336431,31.2638292832001,208.75));
#24718=CARTESIAN_POINT('',(-10.9804588336431,31.2638292832001,208.75));
#24719=CARTESIAN_POINT('Origin',(-11.7304588336431,31.2638292832001,208.75));
#24720=CARTESIAN_POINT('',(-6.98045883364311,31.2638292832001,208.75));
#24721=CARTESIAN_POINT('Origin',(-7.73045883364311,31.2638292832001,208.75));
#24722=CARTESIAN_POINT('',(-2.9804588336431,31.2638292832,208.75));
#24723=CARTESIAN_POINT('Origin',(-3.7304588336431,31.2638292832,208.75));
#24724=CARTESIAN_POINT('',(1.01954116635688,31.2638292832,208.75));
#24725=CARTESIAN_POINT('Origin',(0.269541166356885,31.2638292832,208.75));
#24726=CARTESIAN_POINT('',(5.01954116635689,31.2638292831999,208.75));
#24727=CARTESIAN_POINT('Origin',(4.26954116635689,31.2638292831999,208.75));
#24728=CARTESIAN_POINT('',(9.01954116635689,31.2638292831999,208.75));
#24729=CARTESIAN_POINT('Origin',(8.26954116635689,31.2638292831999,208.75));
#24730=CARTESIAN_POINT('',(13.0195411663569,31.2638292831998,208.75));
#24731=CARTESIAN_POINT('Origin',(12.2695411663569,31.2638292831999,208.75));
#24732=CARTESIAN_POINT('',(17.0195411663569,31.2638292831998,208.75));
#24733=CARTESIAN_POINT('Origin',(16.2695411663569,31.2638292831998,208.75));
#24734=CARTESIAN_POINT('Origin',(17.369541166357,31.2638292831998,198.2));
#24735=CARTESIAN_POINT('',(17.369541166357,31.2638292831998,201.55));
#24736=CARTESIAN_POINT('',(17.3695411663569,31.2638292831998,204.95));
#24737=CARTESIAN_POINT('Origin',(16.2695411663569,31.2638292831998,208.75));
#24738=CARTESIAN_POINT('',(17.0195411663569,31.2638292831998,208.75));
#24739=CARTESIAN_POINT('Origin',(12.2695411663569,31.2638292831999,208.75));
#24740=CARTESIAN_POINT('',(13.0195411663569,31.2638292831998,208.75));
#24741=CARTESIAN_POINT('Origin',(8.26954116635689,31.2638292831999,208.75));
#24742=CARTESIAN_POINT('',(9.01954116635689,31.2638292831999,208.75));
#24743=CARTESIAN_POINT('Origin',(4.26954116635689,31.2638292831999,208.75));
#24744=CARTESIAN_POINT('',(5.01954116635689,31.2638292831999,208.75));
#24745=CARTESIAN_POINT('Origin',(0.269541166356885,31.2638292832,208.75));
#24746=CARTESIAN_POINT('',(1.01954116635688,31.2638292832,208.75));
#24747=CARTESIAN_POINT('Origin',(-3.7304588336431,31.2638292832,208.75));
#24748=CARTESIAN_POINT('',(-2.9804588336431,31.2638292832,208.75));
#24749=CARTESIAN_POINT('Origin',(-7.73045883364311,31.2638292832001,208.75));
#24750=CARTESIAN_POINT('',(-6.98045883364311,31.2638292832001,208.75));
#24751=CARTESIAN_POINT('Origin',(-11.7304588336431,31.2638292832001,208.75));
#24752=CARTESIAN_POINT('',(-10.9804588336431,31.2638292832001,208.75));
#24753=CARTESIAN_POINT('Origin',(-15.7304588336431,31.2638292832001,208.75));
#24754=CARTESIAN_POINT('',(-14.9804588336431,31.2638292832001,208.75));
#24755=CARTESIAN_POINT('Origin',(-19.7304588336431,31.2638292832002,208.75));
#24756=CARTESIAN_POINT('',(-18.9804588336431,31.2638292832002,208.75));
#24757=CARTESIAN_POINT('Origin',(-23.7304588336431,31.2638292832002,208.75));
#24758=CARTESIAN_POINT('',(-22.9804588336431,31.2638292832002,208.75));
#24759=CARTESIAN_POINT('Origin',(-27.7304588336431,31.2638292832003,208.75));
#24760=CARTESIAN_POINT('',(-26.9804588336431,31.2638292832002,208.75));
#24761=CARTESIAN_POINT('Origin',(-31.7304588336431,31.2638292832003,208.75));
#24762=CARTESIAN_POINT('',(-30.9804588336431,31.2638292832003,208.75));
#24763=CARTESIAN_POINT('Origin',(-35.7304588336431,31.2638292832003,208.75));
#24764=CARTESIAN_POINT('',(-34.9804588336431,31.2638292832003,208.75));
#24765=CARTESIAN_POINT('Origin',(-39.7304588336431,31.2638292832004,208.75));
#24766=CARTESIAN_POINT('',(-38.9804588336431,31.2638292832004,208.75));
#24767=CARTESIAN_POINT('Origin',(-43.7304588336431,31.2638292832004,208.75));
#24768=CARTESIAN_POINT('',(-42.9804588336431,31.2638292832004,208.75));
#24769=CARTESIAN_POINT('Origin',(-47.7304588336431,31.2638292832005,208.75));
#24770=CARTESIAN_POINT('',(-46.9804588336431,31.2638292832004,208.75));
#24771=CARTESIAN_POINT('Origin',(-51.7304588336431,31.2638292832005,208.749999999999));
#24772=CARTESIAN_POINT('',(-50.9804588336431,31.2638292832005,208.749999999999));
#24773=CARTESIAN_POINT('Origin',(-55.7304588336431,31.2638292832005,208.749999999999));
#24774=CARTESIAN_POINT('',(-54.9804588336431,31.2638292832005,208.749999999999));
#24775=CARTESIAN_POINT('Origin',(-59.7304588336431,31.2638292832006,208.749999999999));
#24776=CARTESIAN_POINT('',(-58.9804588336431,31.2638292832006,208.749999999999));
#24777=CARTESIAN_POINT('Origin',(-63.7304588336431,31.2638292832006,208.749999999999));
#24778=CARTESIAN_POINT('',(-62.9804588336431,31.2638292832006,208.749999999999));
#24779=CARTESIAN_POINT('Origin',(-67.7304588336431,31.2638292832007,208.749999999999));
#24780=CARTESIAN_POINT('',(-66.9804588336431,31.2638292832006,208.749999999999));
#24781=CARTESIAN_POINT('Origin',(-71.7304588336431,31.2638292832007,208.749999999999));
#24782=CARTESIAN_POINT('',(-70.9804588336431,31.2638292832007,208.749999999999));
#24783=CARTESIAN_POINT('Origin',(-75.7304588336431,31.2638292832007,208.749999999999));
#24784=CARTESIAN_POINT('',(-74.9804588336431,31.2638292832007,208.749999999999));
#24785=CARTESIAN_POINT('Origin',(-79.7304588336431,31.2638292832008,208.749999999999));
#24786=CARTESIAN_POINT('',(-78.9804588336431,31.2638292832008,208.749999999999));
#24787=CARTESIAN_POINT('Origin',(-83.7304588336431,31.2638292832008,208.749999999999));
#24788=CARTESIAN_POINT('',(-82.9804588336431,31.2638292832008,208.749999999999));
#24789=CARTESIAN_POINT('Origin',(-82.630458833643,31.2638292832008,198.199999999999));
#24790=CARTESIAN_POINT('',(-82.630458833643,31.2638292832008,201.549999999999));
#24791=CARTESIAN_POINT('',(-82.6304588336431,31.2638292832008,204.949999999999));
#24792=CARTESIAN_POINT('Origin',(-78.630458833643,31.2638292832008,198.199999999999));
#24793=CARTESIAN_POINT('',(-78.630458833643,31.2638292832008,201.549999999999));
#24794=CARTESIAN_POINT('',(-78.6304588336431,31.2638292832008,204.949999999999));
#24795=CARTESIAN_POINT('Origin',(-74.630458833643,31.2638292832007,198.199999999999));
#24796=CARTESIAN_POINT('',(-74.630458833643,31.2638292832007,201.549999999999));
#24797=CARTESIAN_POINT('',(-74.6304588336431,31.2638292832007,204.949999999999));
#24798=CARTESIAN_POINT('Origin',(-70.630458833643,31.2638292832007,198.199999999999));
#24799=CARTESIAN_POINT('',(-70.630458833643,31.2638292832007,201.549999999999));
#24800=CARTESIAN_POINT('',(-70.6304588336431,31.2638292832007,204.949999999999));
#24801=CARTESIAN_POINT('Origin',(-66.630458833643,31.2638292832006,198.199999999999));
#24802=CARTESIAN_POINT('',(-66.630458833643,31.2638292832006,201.549999999999));
#24803=CARTESIAN_POINT('',(-66.6304588336431,31.2638292832006,204.949999999999));
#24804=CARTESIAN_POINT('Origin',(-62.630458833643,31.2638292832006,198.199999999999));
#24805=CARTESIAN_POINT('',(-62.6304588336431,31.2638292832006,201.549999999999));
#24806=CARTESIAN_POINT('',(-62.6304588336431,31.2638292832006,204.949999999999));
#24807=CARTESIAN_POINT('Origin',(-58.630458833643,31.2638292832006,198.199999999999));
#24808=CARTESIAN_POINT('',(-58.630458833643,31.2638292832006,201.549999999999));
#24809=CARTESIAN_POINT('',(-58.6304588336431,31.2638292832006,204.949999999999));
#24810=CARTESIAN_POINT('Origin',(-54.630458833643,31.2638292832005,198.199999999999));
#24811=CARTESIAN_POINT('',(-54.630458833643,31.2638292832005,201.549999999999));
#24812=CARTESIAN_POINT('',(-54.6304588336431,31.2638292832005,204.949999999999));
#24813=CARTESIAN_POINT('Origin',(-50.630458833643,31.2638292832005,198.2));
#24814=CARTESIAN_POINT('',(-50.630458833643,31.2638292832005,201.549999999999));
#24815=CARTESIAN_POINT('',(-50.6304588336431,31.2638292832005,204.95));
#24816=CARTESIAN_POINT('Origin',(-46.630458833643,31.2638292832004,198.2));
#24817=CARTESIAN_POINT('',(-46.630458833643,31.2638292832004,201.55));
#24818=CARTESIAN_POINT('',(-46.6304588336431,31.2638292832004,204.95));
#24819=CARTESIAN_POINT('Origin',(-42.630458833643,31.2638292832004,198.2));
#24820=CARTESIAN_POINT('',(-42.630458833643,31.2638292832004,201.55));
#24821=CARTESIAN_POINT('',(-42.6304588336431,31.2638292832004,204.95));
#24822=CARTESIAN_POINT('Origin',(-38.630458833643,31.2638292832004,198.2));
#24823=CARTESIAN_POINT('',(-38.630458833643,31.2638292832004,201.55));
#24824=CARTESIAN_POINT('',(-38.6304588336431,31.2638292832004,204.95));
#24825=CARTESIAN_POINT('Origin',(-34.630458833643,31.2638292832003,198.2));
#24826=CARTESIAN_POINT('',(-34.630458833643,31.2638292832003,201.55));
#24827=CARTESIAN_POINT('',(-34.6304588336431,31.2638292832003,204.95));
#24828=CARTESIAN_POINT('Origin',(-30.630458833643,31.2638292832003,198.2));
#24829=CARTESIAN_POINT('',(-30.630458833643,31.2638292832003,201.55));
#24830=CARTESIAN_POINT('',(-30.6304588336431,31.2638292832003,204.95));
#24831=CARTESIAN_POINT('Origin',(-26.630458833643,31.2638292832002,198.2));
#24832=CARTESIAN_POINT('',(-26.630458833643,31.2638292832002,201.55));
#24833=CARTESIAN_POINT('',(-26.6304588336431,31.2638292832002,204.95));
#24834=CARTESIAN_POINT('Origin',(-22.630458833643,31.2638292832002,198.2));
#24835=CARTESIAN_POINT('',(-22.630458833643,31.2638292832002,201.55));
#24836=CARTESIAN_POINT('',(-22.6304588336431,31.2638292832002,204.95));
#24837=CARTESIAN_POINT('Origin',(-18.630458833643,31.2638292832002,198.2));
#24838=CARTESIAN_POINT('',(-18.630458833643,31.2638292832002,201.55));
#24839=CARTESIAN_POINT('',(-18.6304588336431,31.2638292832002,204.95));
#24840=CARTESIAN_POINT('Origin',(-14.630458833643,31.2638292832001,198.2));
#24841=CARTESIAN_POINT('',(-14.630458833643,31.2638292832001,201.55));
#24842=CARTESIAN_POINT('',(-14.6304588336431,31.2638292832001,204.95));
#24843=CARTESIAN_POINT('Origin',(-10.630458833643,31.2638292832001,198.2));
#24844=CARTESIAN_POINT('',(-10.630458833643,31.2638292832001,201.55));
#24845=CARTESIAN_POINT('',(-10.6304588336431,31.2638292832001,204.95));
#24846=CARTESIAN_POINT('Origin',(-6.63045883364299,31.2638292832,198.2));
#24847=CARTESIAN_POINT('',(-6.63045883364302,31.2638292832,201.55));
#24848=CARTESIAN_POINT('',(-6.63045883364306,31.2638292832,204.95));
#24849=CARTESIAN_POINT('Origin',(-2.630458833643,31.2638292832,198.2));
#24850=CARTESIAN_POINT('',(-2.63045883364303,31.2638292832,201.55));
#24851=CARTESIAN_POINT('',(-2.63045883364307,31.2638292832,204.95));
#24852=CARTESIAN_POINT('Origin',(1.369541166357,31.2638292832,198.2));
#24853=CARTESIAN_POINT('',(1.36954116635697,31.2638292832,201.55));
#24854=CARTESIAN_POINT('',(1.36954116635693,31.2638292832,204.95));
#24855=CARTESIAN_POINT('Origin',(5.369541166357,31.2638292831999,198.2));
#24856=CARTESIAN_POINT('',(5.36954116635698,31.2638292831999,201.55));
#24857=CARTESIAN_POINT('',(5.36954116635693,31.2638292831999,204.95));
#24858=CARTESIAN_POINT('Origin',(9.36954116635701,31.2638292831999,198.2));
#24859=CARTESIAN_POINT('',(9.36954116635698,31.2638292831999,201.55));
#24860=CARTESIAN_POINT('',(9.36954116635694,31.2638292831999,204.95));
#24861=CARTESIAN_POINT('Origin',(13.369541166357,31.2638292831998,198.2));
#24862=CARTESIAN_POINT('',(13.369541166357,31.2638292831998,201.55));
#24863=CARTESIAN_POINT('',(13.3695411663569,31.2638292831998,204.95));
#24864=CARTESIAN_POINT('Origin',(-101.730458833643,31.263829283201,210.499999999999));
#24865=CARTESIAN_POINT('',(-85.6069914720345,31.2638292832008,210.499999999999));
#24866=CARTESIAN_POINT('',(18.2695411663569,31.2638292831998,210.5));
#24867=CARTESIAN_POINT('Origin',(18.269541166357,31.2638292831998,198.2));
#24868=CARTESIAN_POINT('',(18.269541166357,31.2638292831998,198.2));
#24869=CARTESIAN_POINT('Origin',(-101.730458833643,31.263829283201,198.199999999999));
#24870=CARTESIAN_POINT('',(-85.6069914720345,31.2638292832008,198.199999999999));
#24871=CARTESIAN_POINT('Origin',(-101.730458833643,31.263829283201,204.949999999999));
#24872=CARTESIAN_POINT('',(-84.8304588336431,31.2638292832008,204.949999999999));
#24873=CARTESIAN_POINT('Origin',(-84.830458833643,31.2638292832008,198.199999999999));
#24874=CARTESIAN_POINT('',(-84.830458833643,31.2638292832008,201.549999999999));
#24875=CARTESIAN_POINT('Origin',(-101.730458833643,31.263829283201,201.549999999999));
#24876=CARTESIAN_POINT('Origin',(-101.730458833643,31.263829283201,204.949999999999));
#24877=CARTESIAN_POINT('',(-80.8304588336431,31.2638292832008,204.949999999999));
#24878=CARTESIAN_POINT('Origin',(-80.830458833643,31.2638292832008,198.199999999999));
#24879=CARTESIAN_POINT('',(-80.830458833643,31.2638292832008,201.549999999999));
#24880=CARTESIAN_POINT('Origin',(-101.730458833643,31.263829283201,201.549999999999));
#24881=CARTESIAN_POINT('Origin',(-101.730458833643,31.263829283201,204.949999999999));
#24882=CARTESIAN_POINT('',(-76.8304588336431,31.2638292832007,204.949999999999));
#24883=CARTESIAN_POINT('Origin',(-76.830458833643,31.2638292832007,198.199999999999));
#24884=CARTESIAN_POINT('',(-76.830458833643,31.2638292832007,201.549999999999));
#24885=CARTESIAN_POINT('Origin',(-101.730458833643,31.263829283201,201.549999999999));
#24886=CARTESIAN_POINT('Origin',(-101.730458833643,31.263829283201,204.949999999999));
#24887=CARTESIAN_POINT('',(-72.8304588336431,31.2638292832007,204.949999999999));
#24888=CARTESIAN_POINT('Origin',(-72.830458833643,31.2638292832007,198.199999999999));
#24889=CARTESIAN_POINT('',(-72.830458833643,31.2638292832007,201.549999999999));
#24890=CARTESIAN_POINT('Origin',(-101.730458833643,31.263829283201,201.549999999999));
#24891=CARTESIAN_POINT('Origin',(-101.730458833643,31.263829283201,204.949999999999));
#24892=CARTESIAN_POINT('',(-68.8304588336431,31.2638292832007,204.949999999999));
#24893=CARTESIAN_POINT('Origin',(-68.830458833643,31.2638292832007,198.199999999999));
#24894=CARTESIAN_POINT('',(-68.830458833643,31.2638292832007,201.549999999999));
#24895=CARTESIAN_POINT('Origin',(-101.730458833643,31.263829283201,201.549999999999));
#24896=CARTESIAN_POINT('Origin',(-101.730458833643,31.263829283201,204.949999999999));
#24897=CARTESIAN_POINT('',(-64.8304588336431,31.2638292832006,204.949999999999));
#24898=CARTESIAN_POINT('Origin',(-64.830458833643,31.2638292832006,198.199999999999));
#24899=CARTESIAN_POINT('',(-64.830458833643,31.2638292832006,201.549999999999));
#24900=CARTESIAN_POINT('Origin',(-101.730458833643,31.263829283201,201.549999999999));
#24901=CARTESIAN_POINT('Origin',(-101.730458833643,31.263829283201,204.949999999999));
#24902=CARTESIAN_POINT('',(-60.8304588336431,31.2638292832006,204.949999999999));
#24903=CARTESIAN_POINT('Origin',(-60.830458833643,31.2638292832006,198.199999999999));
#24904=CARTESIAN_POINT('',(-60.830458833643,31.2638292832006,201.549999999999));
#24905=CARTESIAN_POINT('Origin',(-101.730458833643,31.263829283201,201.549999999999));
#24906=CARTESIAN_POINT('Origin',(-101.730458833643,31.263829283201,204.949999999999));
#24907=CARTESIAN_POINT('',(-56.8304588336431,31.2638292832006,204.949999999999));
#24908=CARTESIAN_POINT('Origin',(-56.830458833643,31.2638292832006,198.199999999999));
#24909=CARTESIAN_POINT('',(-56.830458833643,31.2638292832006,201.549999999999));
#24910=CARTESIAN_POINT('Origin',(-101.730458833643,31.263829283201,201.549999999999));
#24911=CARTESIAN_POINT('Origin',(-101.730458833643,31.263829283201,204.949999999999));
#24912=CARTESIAN_POINT('',(-52.8304588336431,31.2638292832005,204.949999999999));
#24913=CARTESIAN_POINT('Origin',(-52.830458833643,31.2638292832005,198.2));
#24914=CARTESIAN_POINT('',(-52.830458833643,31.2638292832005,201.549999999999));
#24915=CARTESIAN_POINT('Origin',(-101.730458833643,31.263829283201,201.549999999999));
#24916=CARTESIAN_POINT('Origin',(-101.730458833643,31.263829283201,204.949999999999));
#24917=CARTESIAN_POINT('',(-48.8304588336431,31.2638292832005,204.95));
#24918=CARTESIAN_POINT('Origin',(-48.830458833643,31.2638292832005,198.2));
#24919=CARTESIAN_POINT('',(-48.830458833643,31.2638292832005,201.549999999999));
#24920=CARTESIAN_POINT('Origin',(-101.730458833643,31.263829283201,201.549999999999));
#24921=CARTESIAN_POINT('Origin',(-101.730458833643,31.263829283201,204.949999999999));
#24922=CARTESIAN_POINT('',(-44.8304588336431,31.2638292832004,204.95));
#24923=CARTESIAN_POINT('Origin',(-44.830458833643,31.2638292832004,198.2));
#24924=CARTESIAN_POINT('',(-44.830458833643,31.2638292832004,201.55));
#24925=CARTESIAN_POINT('Origin',(-101.730458833643,31.263829283201,201.549999999999));
#24926=CARTESIAN_POINT('Origin',(-101.730458833643,31.263829283201,204.949999999999));
#24927=CARTESIAN_POINT('',(-40.8304588336431,31.2638292832004,204.95));
#24928=CARTESIAN_POINT('Origin',(-40.830458833643,31.2638292832004,198.2));
#24929=CARTESIAN_POINT('',(-40.830458833643,31.2638292832004,201.55));
#24930=CARTESIAN_POINT('Origin',(-101.730458833643,31.263829283201,201.549999999999));
#24931=CARTESIAN_POINT('Origin',(-101.730458833643,31.263829283201,204.949999999999));
#24932=CARTESIAN_POINT('',(-36.8304588336431,31.2638292832004,204.95));
#24933=CARTESIAN_POINT('Origin',(-36.830458833643,31.2638292832004,198.2));
#24934=CARTESIAN_POINT('',(-36.830458833643,31.2638292832004,201.55));
#24935=CARTESIAN_POINT('Origin',(-101.730458833643,31.263829283201,201.549999999999));
#24936=CARTESIAN_POINT('Origin',(-101.730458833643,31.263829283201,204.949999999999));
#24937=CARTESIAN_POINT('',(-32.8304588336431,31.2638292832003,204.95));
#24938=CARTESIAN_POINT('Origin',(-32.830458833643,31.2638292832003,198.2));
#24939=CARTESIAN_POINT('',(-32.830458833643,31.2638292832003,201.55));
#24940=CARTESIAN_POINT('Origin',(-101.730458833643,31.263829283201,201.549999999999));
#24941=CARTESIAN_POINT('Origin',(-101.730458833643,31.263829283201,204.949999999999));
#24942=CARTESIAN_POINT('',(-28.8304588336431,31.2638292832003,204.95));
#24943=CARTESIAN_POINT('Origin',(-28.830458833643,31.2638292832003,198.2));
#24944=CARTESIAN_POINT('',(-28.830458833643,31.2638292832003,201.55));
#24945=CARTESIAN_POINT('Origin',(-101.730458833643,31.263829283201,201.549999999999));
#24946=CARTESIAN_POINT('Origin',(-101.730458833643,31.263829283201,204.949999999999));
#24947=CARTESIAN_POINT('',(-24.8304588336431,31.2638292832002,204.95));
#24948=CARTESIAN_POINT('Origin',(-24.830458833643,31.2638292832002,198.2));
#24949=CARTESIAN_POINT('',(-24.830458833643,31.2638292832002,201.55));
#24950=CARTESIAN_POINT('Origin',(-101.730458833643,31.263829283201,201.549999999999));
#24951=CARTESIAN_POINT('Origin',(-101.730458833643,31.263829283201,204.949999999999));
#24952=CARTESIAN_POINT('',(-20.8304588336431,31.2638292832002,204.95));
#24953=CARTESIAN_POINT('Origin',(-20.830458833643,31.2638292832002,198.2));
#24954=CARTESIAN_POINT('',(-20.830458833643,31.2638292832002,201.55));
#24955=CARTESIAN_POINT('Origin',(-101.730458833643,31.263829283201,201.549999999999));
#24956=CARTESIAN_POINT('Origin',(-101.730458833643,31.263829283201,204.949999999999));
#24957=CARTESIAN_POINT('',(-16.8304588336431,31.2638292832002,204.95));
#24958=CARTESIAN_POINT('Origin',(-16.830458833643,31.2638292832002,198.2));
#24959=CARTESIAN_POINT('',(-16.830458833643,31.2638292832002,201.55));
#24960=CARTESIAN_POINT('Origin',(-101.730458833643,31.263829283201,201.549999999999));
#24961=CARTESIAN_POINT('Origin',(-101.730458833643,31.263829283201,204.949999999999));
#24962=CARTESIAN_POINT('',(-12.8304588336431,31.2638292832001,204.95));
#24963=CARTESIAN_POINT('Origin',(-12.830458833643,31.2638292832001,198.2));
#24964=CARTESIAN_POINT('',(-12.830458833643,31.2638292832001,201.55));
#24965=CARTESIAN_POINT('Origin',(-101.730458833643,31.263829283201,201.549999999999));
#24966=CARTESIAN_POINT('Origin',(-101.730458833643,31.263829283201,204.949999999999));
#24967=CARTESIAN_POINT('',(-8.83045883364307,31.2638292832001,204.95));
#24968=CARTESIAN_POINT('Origin',(-8.830458833643,31.2638292832001,198.2));
#24969=CARTESIAN_POINT('',(-8.83045883364303,31.2638292832001,201.55));
#24970=CARTESIAN_POINT('Origin',(-101.730458833643,31.263829283201,201.549999999999));
#24971=CARTESIAN_POINT('Origin',(-101.730458833643,31.263829283201,204.949999999999));
#24972=CARTESIAN_POINT('',(-4.83045883364307,31.2638292832,204.95));
#24973=CARTESIAN_POINT('Origin',(-4.830458833643,31.2638292832,198.2));
#24974=CARTESIAN_POINT('',(-4.83045883364302,31.2638292832,201.55));
#24975=CARTESIAN_POINT('Origin',(-101.730458833643,31.263829283201,201.549999999999));
#24976=CARTESIAN_POINT('Origin',(-101.730458833643,31.263829283201,204.949999999999));
#24977=CARTESIAN_POINT('',(-0.830458833643063,31.2638292832,204.95));
#24978=CARTESIAN_POINT('Origin',(-0.830458833642994,31.2638292832,198.2));
#24979=CARTESIAN_POINT('',(-0.830458833643022,31.2638292832,201.55));
#24980=CARTESIAN_POINT('Origin',(-101.730458833643,31.263829283201,201.549999999999));
#24981=CARTESIAN_POINT('Origin',(-101.730458833643,31.263829283201,204.949999999999));
#24982=CARTESIAN_POINT('',(3.16954116635693,31.2638292832,204.95));
#24983=CARTESIAN_POINT('Origin',(3.169541166357,31.2638292832,198.2));
#24984=CARTESIAN_POINT('',(3.16954116635697,31.2638292832,201.55));
#24985=CARTESIAN_POINT('Origin',(-101.730458833643,31.263829283201,201.549999999999));
#24986=CARTESIAN_POINT('Origin',(-101.730458833643,31.263829283201,204.949999999999));
#24987=CARTESIAN_POINT('',(7.16954116635693,31.2638292831999,204.95));
#24988=CARTESIAN_POINT('Origin',(7.169541166357,31.2638292831999,198.2));
#24989=CARTESIAN_POINT('',(7.16954116635697,31.2638292831999,201.55));
#24990=CARTESIAN_POINT('Origin',(-101.730458833643,31.263829283201,201.549999999999));
#24991=CARTESIAN_POINT('Origin',(-101.730458833643,31.263829283201,204.949999999999));
#24992=CARTESIAN_POINT('',(11.1695411663569,31.2638292831999,204.95));
#24993=CARTESIAN_POINT('Origin',(11.169541166357,31.2638292831999,198.2));
#24994=CARTESIAN_POINT('',(11.169541166357,31.2638292831999,201.55));
#24995=CARTESIAN_POINT('Origin',(-101.730458833643,31.263829283201,201.549999999999));
#24996=CARTESIAN_POINT('Origin',(-101.730458833643,31.263829283201,204.949999999999));
#24997=CARTESIAN_POINT('',(15.1695411663569,31.2638292831998,204.95));
#24998=CARTESIAN_POINT('Origin',(15.169541166357,31.2638292831998,198.2));
#24999=CARTESIAN_POINT('',(15.169541166357,31.2638292831998,201.55));
#25000=CARTESIAN_POINT('Origin',(-101.730458833643,31.263829283201,201.549999999999));
#25001=CARTESIAN_POINT('Origin',(-85.6069914720347,10.7638292832008,194.611133062546));
#25002=CARTESIAN_POINT('',(0.,0.,0.));
#25003=CARTESIAN_POINT('Origin',(-31.761699248248,37.153679903937,214.471369141518));
#25004=CARTESIAN_POINT('',(-32.261699248248,37.153679903937,214.471369141518));
#25005=CARTESIAN_POINT('',(-31.761699248248,37.653679903937,213.971369141518));
#25006=CARTESIAN_POINT('Origin',(-31.76169924825,37.1536799039392,213.97136914152));
#25007=CARTESIAN_POINT('',(-31.261699248248,37.153679903937,214.471369141518));
#25008=CARTESIAN_POINT('Origin',(-31.7616992482473,37.1536799039377,213.971369141519));
#25009=CARTESIAN_POINT('',(-31.261699248248,37.153679903937,205.771369141518));
#25010=CARTESIAN_POINT('',(-31.261699248248,37.153679903937,214.471369141518));
#25011=CARTESIAN_POINT('',(-31.761699248248,37.653679903937,206.271369141518));
#25012=CARTESIAN_POINT('Origin',(-31.7616992482484,37.1536799039366,206.271369141519));
#25013=CARTESIAN_POINT('',(-32.261699248248,37.153679903937,205.771369141518));
#25014=CARTESIAN_POINT('Origin',(-31.761699248248,37.1536799039369,206.271369141518));
#25015=CARTESIAN_POINT('',(-32.261699248248,37.153679903937,214.471369141518));
#25016=CARTESIAN_POINT('Origin',(-32.261699248248,37.153679903937,206.271369141518));
#25017=CARTESIAN_POINT('',(-32.261699248248,37.153679903937,205.771369141518));
#25018=CARTESIAN_POINT('Origin',(-32.261699248248,37.153679903937,213.971369141518));
#25019=CARTESIAN_POINT('',(-32.261699248248,37.153679903937,214.471369141518));
#25020=CARTESIAN_POINT('Origin',(1.93830075175198,37.1536799039369,207.844898865397));
#25021=CARTESIAN_POINT('',(1.43830075175198,37.1536799039369,207.844898865397));
#25022=CARTESIAN_POINT('',(1.93830075175198,37.6536799039369,207.344898865397));
#25023=CARTESIAN_POINT('Origin',(1.93830075175113,37.1536799039378,207.344898865398));
#25024=CARTESIAN_POINT('',(2.43830075175198,37.1536799039369,207.844898865397));
#25025=CARTESIAN_POINT('Origin',(1.93830075175171,37.1536799039367,207.344898865397));
#25026=CARTESIAN_POINT('',(2.43830075175197,37.1536799039369,198.5));
#25027=CARTESIAN_POINT('',(2.43830075175198,37.1536799039369,207.844898865397));
#25028=CARTESIAN_POINT('',(1.93830075175197,37.6536799039369,199.));
#25029=CARTESIAN_POINT('Origin',(1.93830075175225,37.1536799039372,199.));
#25030=CARTESIAN_POINT('',(1.43830075175197,37.1536799039369,198.5));
#25031=CARTESIAN_POINT('Origin',(1.93830075175189,37.153679903937,199.));
#25032=CARTESIAN_POINT('',(1.43830075175198,37.1536799039369,207.844898865397));
#25033=CARTESIAN_POINT('Origin',(-69.261699248248,37.153679903937,199.));
#25034=CARTESIAN_POINT('',(-69.261699248248,37.153679903937,198.5));
#25035=CARTESIAN_POINT('Origin',(1.43830075175198,37.1536799039369,207.344898865397));
#25036=CARTESIAN_POINT('',(1.43830075175198,37.1536799039369,207.844898865397));
#25037=CARTESIAN_POINT('Origin',(1.938300751752,37.1536799039369,214.501561642103));
#25038=CARTESIAN_POINT('',(1.438300751752,37.1536799039369,214.501561642103));
#25039=CARTESIAN_POINT('',(1.938300751752,37.6536799039369,214.001561642103));
#25040=CARTESIAN_POINT('Origin',(1.93830075175188,37.1536799039369,214.001561642103));
#25041=CARTESIAN_POINT('',(2.438300751752,37.1536799039369,214.501561642103));
#25042=CARTESIAN_POINT('Origin',(1.93830075175259,37.1536799039376,214.001561642104));
#25043=CARTESIAN_POINT('',(2.43830075175199,37.1536799039369,209.344898865397));
#25044=CARTESIAN_POINT('',(2.438300751752,37.1536799039369,214.501561642103));
#25045=CARTESIAN_POINT('',(1.93830075175199,37.6536799039369,209.844898865397));
#25046=CARTESIAN_POINT('Origin',(1.93830075175128,37.1536799039362,209.844898865398));
#25047=CARTESIAN_POINT('',(1.43830075175199,37.1536799039369,209.344898865397));
#25048=CARTESIAN_POINT('Origin',(1.93830075175241,37.1536799039365,209.844898865398));
#25049=CARTESIAN_POINT('',(1.438300751752,37.1536799039369,214.501561642103));
#25050=CARTESIAN_POINT('Origin',(1.43830075175199,37.1536799039369,209.844898865397));
#25051=CARTESIAN_POINT('',(1.43830075175199,37.1536799039369,209.344898865397));
#25052=CARTESIAN_POINT('Origin',(1.438300751752,37.1536799039369,214.001561642103));
#25053=CARTESIAN_POINT('',(1.438300751752,37.1536799039369,214.501561642103));
#25054=CARTESIAN_POINT('Ctrl Pts',(-69.761699248248,33.353679903937,209.3));
#25055=CARTESIAN_POINT('Ctrl Pts',(-69.761699248248,32.853679903937,209.3));
#25056=CARTESIAN_POINT('Ctrl Pts',(-69.261699248248,32.853679903937,209.3));
#25057=CARTESIAN_POINT('Ctrl Pts',(-70.261699248248,33.353679903937,209.3));
#25058=CARTESIAN_POINT('Ctrl Pts',(-70.261699248248,32.353679903937,209.3));
#25059=CARTESIAN_POINT('Ctrl Pts',(-69.261699248248,32.353679903937,209.3));
#25060=CARTESIAN_POINT('Ctrl Pts',(-70.261699248248,33.353679903937,209.8));
#25061=CARTESIAN_POINT('Ctrl Pts',(-70.261699248248,32.353679903937,209.8));
#25062=CARTESIAN_POINT('Ctrl Pts',(-69.261699248248,32.353679903937,209.8));
#25063=CARTESIAN_POINT('',(-69.261699248248,32.353679903937,209.8));
#25064=CARTESIAN_POINT('',(-69.261699248248,32.853679903937,209.3));
#25065=CARTESIAN_POINT('Origin',(-69.261699248248,32.853679903937,209.8));
#25066=CARTESIAN_POINT('',(-70.261699248248,33.353679903937,209.8));
#25067=CARTESIAN_POINT('Origin',(-69.261699248248,33.353679903937,209.8));
#25068=CARTESIAN_POINT('',(-69.761699248248,33.353679903937,209.3));
#25069=CARTESIAN_POINT('Origin',(-69.761699248248,33.353679903937,209.8));
#25070=CARTESIAN_POINT('Origin',(-69.261699248248,33.353679903937,209.3));
#25071=CARTESIAN_POINT('Origin',(-69.761699248248,33.353679903937,209.8));
#25072=CARTESIAN_POINT('',(-70.261699248248,35.053679903937,209.8));
#25073=CARTESIAN_POINT('',(-69.261699248248,35.053679903937,209.8));
#25074=CARTESIAN_POINT('Origin',(-69.761699248248,35.053679903937,209.8));
#25075=CARTESIAN_POINT('',(-69.261699248248,33.353679903937,209.8));
#25076=CARTESIAN_POINT('',(-69.261699248248,35.553679903937,209.8));
#25077=CARTESIAN_POINT('Origin',(-69.761699248248,33.353679903937,209.8));
#25078=CARTESIAN_POINT('',(-70.261699248248,33.353679903937,209.8));
#25079=CARTESIAN_POINT('Origin',(-69.761699248248,35.053679903937,209.8));
#25080=CARTESIAN_POINT('Origin',(-69.761699248248,35.053679903937,209.8));
#25081=CARTESIAN_POINT('Origin',(-69.761699248248,35.053679903937,215.5));
#25082=CARTESIAN_POINT('',(-70.261699248248,35.053679903937,214.));
#25083=CARTESIAN_POINT('',(-69.261699248248,35.053679903937,214.));
#25084=CARTESIAN_POINT('Origin',(-69.761699248248,35.053679903937,214.));
#25085=CARTESIAN_POINT('',(-69.261699248248,35.053679903937,213.325088768032));
#25086=CARTESIAN_POINT('',(-69.261699248248,35.053679903937,209.3));
#25087=CARTESIAN_POINT('',(-69.261699248248,35.053679903937,210.465382311583));
#25088=CARTESIAN_POINT('',(-69.261699248248,35.053679903937,209.3));
#25089=CARTESIAN_POINT('',(-69.261699248248,35.053679903937,209.3));
#25090=CARTESIAN_POINT('',(-70.261699248248,35.053679903937,210.465382311583));
#25091=CARTESIAN_POINT('',(-70.261699248248,35.053679903937,209.8));
#25092=CARTESIAN_POINT('',(-70.261699248248,35.053679903937,213.325088768032));
#25093=CARTESIAN_POINT('',(-70.261699248248,35.053679903937,209.965382311583));
#25094=CARTESIAN_POINT('',(-70.261699248248,35.053679903937,209.8));
#25095=CARTESIAN_POINT('Origin',(-69.761699248248,35.053679903937,214.));
#25096=CARTESIAN_POINT('Origin',(-69.761699248248,35.053679903937,214.));
#25097=CARTESIAN_POINT('Origin',(-69.761699248248,33.353679903937,214.));
#25098=CARTESIAN_POINT('',(-70.261699248248,33.353679903937,214.));
#25099=CARTESIAN_POINT('',(-69.761699248248,33.353679903937,214.5));
#25100=CARTESIAN_POINT('Origin',(-69.761699248248,33.353679903937,214.));
#25101=CARTESIAN_POINT('',(-69.261699248248,33.353679903937,214.));
#25102=CARTESIAN_POINT('Origin',(-69.761699248248,33.353679903937,214.));
#25103=CARTESIAN_POINT('',(-69.261699248248,35.553679903937,214.));
#25104=CARTESIAN_POINT('',(-70.261699248248,35.053679903937,214.));
#25105=CARTESIAN_POINT('Ctrl Pts',(-69.261699248248,32.853679903937,214.5));
#25106=CARTESIAN_POINT('Ctrl Pts',(-69.761699248248,32.853679903937,214.5));
#25107=CARTESIAN_POINT('Ctrl Pts',(-69.761699248248,33.353679903937,214.5));
#25108=CARTESIAN_POINT('Ctrl Pts',(-69.261699248248,32.353679903937,214.5));
#25109=CARTESIAN_POINT('Ctrl Pts',(-70.261699248248,32.353679903937,214.5));
#25110=CARTESIAN_POINT('Ctrl Pts',(-70.261699248248,33.353679903937,214.5));
#25111=CARTESIAN_POINT('Ctrl Pts',(-69.261699248248,32.353679903937,214.));
#25112=CARTESIAN_POINT('Ctrl Pts',(-70.261699248248,32.353679903937,214.));
#25113=CARTESIAN_POINT('Ctrl Pts',(-70.261699248248,33.353679903937,214.));
#25114=CARTESIAN_POINT('',(-69.261699248248,32.353679903937,214.));
#25115=CARTESIAN_POINT('',(-69.261699248248,32.3608987452201,214.084656539108));
#25116=CARTESIAN_POINT('Origin',(-69.261699248248,32.853679903937,214.));
#25117=CARTESIAN_POINT('',(-69.261699248248,32.853679903937,214.5));
#25118=CARTESIAN_POINT('Origin',(-69.261699248248,32.853679903937,214.));
#25119=CARTESIAN_POINT('Origin',(-69.261699248248,33.353679903937,214.5));
#25120=CARTESIAN_POINT('Origin',(-69.261699248248,33.353679903937,214.));
#25121=CARTESIAN_POINT('Origin',(-70.261699248248,32.853679903937,214.));
#25122=CARTESIAN_POINT('',(-64.261699248248,32.3608987452201,214.084656539108));
#25123=CARTESIAN_POINT('',(-69.261699248248,32.3608987452201,214.084656539108));
#25124=CARTESIAN_POINT('',(-64.261699248248,32.353679903937,214.));
#25125=CARTESIAN_POINT('',(-70.261699248248,32.353679903937,214.));
#25126=CARTESIAN_POINT('Origin',(-64.261699248248,32.853679903937,214.));
#25127=CARTESIAN_POINT('Origin',(-32.561699248248,33.5567577319955,206.621369141518));
#25128=CARTESIAN_POINT('',(-32.261699248248,34.7567577319955,206.621369141518));
#25129=CARTESIAN_POINT('',(-32.261699248248,33.853679903937,206.621369141518));
#25130=CARTESIAN_POINT('',(-32.261699248248,37.653679903937,206.621369141518));
#25131=CARTESIAN_POINT('',(-32.3594092734667,33.5567577319955,206.621369141518));
#25132=CARTESIAN_POINT('Origin',(-32.761699248248,33.853679903937,206.621369141518));
#25133=CARTESIAN_POINT('',(-31.261699248248,33.5567577319955,206.621369141518));
#25134=CARTESIAN_POINT('',(-32.561699248248,33.5567577319955,206.621369141518));
#25135=CARTESIAN_POINT('',(-31.261699248248,34.7567577319955,206.621369141518));
#25136=CARTESIAN_POINT('',(-31.261699248248,33.5567577319955,206.621369141518));
#25137=CARTESIAN_POINT('',(-32.561699248248,34.7567577319955,206.621369141518));
#25138=CARTESIAN_POINT('Origin',(-32.561699248248,34.7567577319955,212.521369141518));
#25139=CARTESIAN_POINT('',(-32.261699248248,34.7567577319955,212.521369141518));
#25140=CARTESIAN_POINT('',(-32.261699248248,34.7567577319955,214.471369141518));
#25141=CARTESIAN_POINT('',(-31.261699248248,34.7567577319955,212.521369141518));
#25142=CARTESIAN_POINT('',(-31.261699248248,34.7567577319955,212.521369141518));
#25143=CARTESIAN_POINT('',(-32.561699248248,34.7567577319955,212.521369141518));
#25144=CARTESIAN_POINT('Origin',(-32.561699248248,36.2479932555265,212.521369141518));
#25145=CARTESIAN_POINT('',(-32.261699248248,36.2479932555265,212.521369141518));
#25146=CARTESIAN_POINT('',(-32.261699248248,37.653679903937,212.521369141518));
#25147=CARTESIAN_POINT('',(-31.261699248248,36.2479932555265,212.521369141518));
#25148=CARTESIAN_POINT('',(-31.261699248248,36.2479932555265,212.521369141518));
#25149=CARTESIAN_POINT('',(-32.561699248248,36.2479932555265,212.521369141518));
#25150=CARTESIAN_POINT('Origin',(-32.561699248248,36.2479932555265,213.621369141518));
#25151=CARTESIAN_POINT('',(-32.261699248248,36.2479932555265,213.621369141518));
#25152=CARTESIAN_POINT('',(-32.261699248248,36.2479932555265,214.471369141518));
#25153=CARTESIAN_POINT('',(-31.261699248248,36.2479932555265,213.621369141518));
#25154=CARTESIAN_POINT('',(-31.261699248248,36.2479932555265,213.621369141518));
#25155=CARTESIAN_POINT('',(-32.561699248248,36.2479932555265,213.621369141518));
#25156=CARTESIAN_POINT('Origin',(-32.561699248248,34.7567577319955,213.621369141518));
#25157=CARTESIAN_POINT('',(-32.261699248248,33.853679903937,213.621369141518));
#25158=CARTESIAN_POINT('',(-32.261699248248,37.653679903937,213.621369141518));
#25159=CARTESIAN_POINT('',(-31.261699248248,33.5567577319955,213.621369141518));
#25160=CARTESIAN_POINT('',(-31.261699248248,34.7567577319955,213.621369141518));
#25161=CARTESIAN_POINT('',(-32.3594092734667,33.5567577319955,213.621369141518));
#25162=CARTESIAN_POINT('',(-32.561699248248,33.5567577319955,213.621369141518));
#25163=CARTESIAN_POINT('Origin',(-32.761699248248,33.853679903937,213.621369141518));
#25164=CARTESIAN_POINT('Origin',(-32.561699248248,33.5567577319955,213.621369141518));
#25165=CARTESIAN_POINT('',(-31.261699248248,33.5567577319955,213.621369141518));
#25166=CARTESIAN_POINT('',(-32.3594092734667,33.5567577319955,214.471369141518));
#25167=CARTESIAN_POINT('Origin',(-31.761699248248,32.853679903937,198.5));
#25168=CARTESIAN_POINT('',(-31.261699248248,32.853679903937,205.771369141518));
#25169=CARTESIAN_POINT('',(-31.761699248248,32.353679903937,205.771369141518));
#25170=CARTESIAN_POINT('Origin',(-31.761699248248,32.853679903937,205.771369141518));
#25171=CARTESIAN_POINT('',(-31.261699248248,32.853679903937,214.471369141518));
#25172=CARTESIAN_POINT('',(-31.261699248248,32.853679903937,214.471369141518));
#25173=CARTESIAN_POINT('',(-31.761699248248,32.353679903937,214.471369141518));
#25174=CARTESIAN_POINT('Origin',(-31.761699248248,32.853679903937,214.471369141518));
#25175=CARTESIAN_POINT('',(-31.761699248248,32.353679903937,198.5));
#25176=CARTESIAN_POINT('Origin',(-32.761699248248,33.853679903937,214.471369141518));
#25177=CARTESIAN_POINT('',(-32.261699248248,33.853679903937,214.471369141518));
#25178=CARTESIAN_POINT('',(-32.261699248248,33.853679903937,214.471369141518));
#25179=CARTESIAN_POINT('',(-32.261699248248,33.853679903937,205.771369141518));
#25180=CARTESIAN_POINT('',(-32.261699248248,33.853679903937,214.471369141518));
#25181=CARTESIAN_POINT('',(-32.761699248248,33.353679903937,205.771369141518));
#25182=CARTESIAN_POINT('Origin',(-32.761699248248,33.853679903937,205.771369141518));
#25183=CARTESIAN_POINT('',(-32.761699248248,33.353679903937,214.471369141518));
#25184=CARTESIAN_POINT('',(-32.761699248248,33.353679903937,205.771369141518));
#25185=CARTESIAN_POINT('Origin',(-32.761699248248,33.853679903937,214.471369141518));
#25186=CARTESIAN_POINT('Origin',(-32.261699248248,37.653679903937,205.771369141518));
#25187=CARTESIAN_POINT('',(-32.261699248248,37.653679903937,205.771369141518));
#25188=CARTESIAN_POINT('',(-31.261699248248,37.653679903937,205.771369141518));
#25189=CARTESIAN_POINT('',(-32.261699248248,32.353679903937,205.771369141518));
#25190=CARTESIAN_POINT('',(-32.261699248248,32.353679903937,205.771369141518));
#25191=CARTESIAN_POINT('',(-32.261699248248,33.353679903937,205.771369141518));
#25192=CARTESIAN_POINT('',(-32.261699248248,32.2748332073222,205.771369141518));
#25193=CARTESIAN_POINT('',(-32.261699248248,33.353679903937,205.771369141518));
#25194=CARTESIAN_POINT('Origin',(-31.261699248248,37.653679903937,214.471369141518));
#25195=CARTESIAN_POINT('',(-31.261699248248,37.653679903937,214.471369141518));
#25196=CARTESIAN_POINT('Origin',(-32.261699248248,37.653679903937,214.471369141518));
#25197=CARTESIAN_POINT('',(-32.261699248248,37.653679903937,214.471369141518));
#25198=CARTESIAN_POINT('',(-32.261699248248,33.353679903937,214.471369141518));
#25199=CARTESIAN_POINT('',(-32.261699248248,33.353679903937,214.471369141518));
#25200=CARTESIAN_POINT('',(-32.261699248248,32.353679903937,214.471369141518));
#25201=CARTESIAN_POINT('',(-32.261699248248,32.2748332073222,214.471369141518));
#25202=CARTESIAN_POINT('',(-32.261699248248,32.353679903937,214.471369141518));
#25203=CARTESIAN_POINT('Origin',(-32.261699248248,37.653679903937,214.471369141518));
#25204=CARTESIAN_POINT('Origin',(1.93830075175196,32.8536799039369,198.5));
#25205=CARTESIAN_POINT('',(2.43830075175198,32.8536799039369,209.344898865397));
#25206=CARTESIAN_POINT('',(1.93830075175198,32.3536799039369,209.344898865397));
#25207=CARTESIAN_POINT('Origin',(1.93830075175198,32.8536799039369,209.344898865397));
#25208=CARTESIAN_POINT('',(2.438300751752,32.8536799039369,214.501561642103));
#25209=CARTESIAN_POINT('',(2.438300751752,32.8536799039369,214.501561642103));
#25210=CARTESIAN_POINT('',(1.938300751752,32.3536799039369,214.501561642103));
#25211=CARTESIAN_POINT('Origin',(1.938300751752,32.8536799039369,214.501561642103));
#25212=CARTESIAN_POINT('',(1.93830075175196,32.3536799039369,198.5));
#25213=CARTESIAN_POINT('Origin',(1.93830075175196,32.8536799039369,198.5));
#25214=CARTESIAN_POINT('',(2.43830075175196,32.8536799039369,198.5));
#25215=CARTESIAN_POINT('',(1.93830075175196,32.3536799039369,198.5));
#25216=CARTESIAN_POINT('Origin',(1.93830075175196,32.8536799039369,198.5));
#25217=CARTESIAN_POINT('',(2.43830075175198,32.8536799039369,207.844898865397));
#25218=CARTESIAN_POINT('',(2.43830075175198,32.8536799039369,207.844898865397));
#25219=CARTESIAN_POINT('',(1.93830075175198,32.3536799039369,207.844898865397));
#25220=CARTESIAN_POINT('Origin',(1.93830075175198,32.8536799039369,207.844898865397));
#25221=CARTESIAN_POINT('',(1.93830075175196,32.3536799039369,198.5));
#25222=CARTESIAN_POINT('Origin',(0.938300751751997,33.8536799039369,214.501561642103));
#25223=CARTESIAN_POINT('',(0.938300751751983,33.3536799039369,209.34762215292));
#25224=CARTESIAN_POINT('',(1.43830075175198,33.8536799039369,209.34762215292));
#25225=CARTESIAN_POINT('Origin',(0.938300751751983,33.8536799039369,209.34762215292));
#25226=CARTESIAN_POINT('',(0.938300751751997,33.3536799039369,214.5));
#25227=CARTESIAN_POINT('',(0.938300751751983,33.3536799039369,209.34762215292));
#25228=CARTESIAN_POINT('',(1.438300751752,33.8536799039369,214.5));
#25229=CARTESIAN_POINT('Origin',(0.938300751751997,33.8536799039369,214.5));
#25230=CARTESIAN_POINT('',(1.438300751752,33.8536799039369,214.5));
#25231=CARTESIAN_POINT('Origin',(0.938300751751983,33.8536799039369,207.844898865397));
#25232=CARTESIAN_POINT('',(0.938300751751962,33.3536799039369,198.5));
#25233=CARTESIAN_POINT('',(1.43830075175196,33.8536799039369,198.5));
#25234=CARTESIAN_POINT('Origin',(0.938300751751962,33.8536799039369,198.5));
#25235=CARTESIAN_POINT('',(0.938300751751983,33.3536799039369,207.844898865397));
#25236=CARTESIAN_POINT('',(0.938300751751962,33.3536799039369,198.5));
#25237=CARTESIAN_POINT('',(1.43830075175198,33.8536799039369,207.844898865397));
#25238=CARTESIAN_POINT('Origin',(0.938300751751983,33.8536799039369,207.844898865397));
#25239=CARTESIAN_POINT('',(1.43830075175198,33.8536799039369,207.844898865397));
#25240=CARTESIAN_POINT('Origin',(-16.261699248248,31.653679903937,209.34762215292));
#25241=CARTESIAN_POINT('',(-13.261699248248,32.3536799039369,209.34762215292));
#25242=CARTESIAN_POINT('',(-16.261699248248,32.353679903937,209.34762215292));
#25243=CARTESIAN_POINT('',(-69.261699248248,32.353679903937,209.34762215292));
#25244=CARTESIAN_POINT('',(-16.261699248248,33.353679903937,209.34762215292));
#25245=CARTESIAN_POINT('',(-16.261699248248,31.653679903937,209.34762215292));
#25246=CARTESIAN_POINT('',(-13.261699248248,33.3536799039369,209.34762215292));
#25247=CARTESIAN_POINT('',(-16.261699248248,33.353679903937,209.34762215292));
#25248=CARTESIAN_POINT('',(-13.261699248248,31.653679903937,209.34762215292));
#25249=CARTESIAN_POINT('Origin',(-13.261699248248,31.653679903937,209.34762215292));
#25250=CARTESIAN_POINT('',(-13.261699248248,32.3536799039369,207.84762215292));
#25251=CARTESIAN_POINT('',(-13.261699248248,32.3536799039369,198.5));
#25252=CARTESIAN_POINT('',(-13.261699248248,33.3536799039369,207.84762215292));
#25253=CARTESIAN_POINT('',(-13.261699248248,33.3536799039369,209.34762215292));
#25254=CARTESIAN_POINT('',(-13.261699248248,31.653679903937,207.84762215292));
#25255=CARTESIAN_POINT('Origin',(-13.261699248248,31.653679903937,207.84762215292));
#25256=CARTESIAN_POINT('',(-16.261699248248,32.353679903937,207.84762215292));
#25257=CARTESIAN_POINT('',(-69.261699248248,32.353679903937,207.84762215292));
#25258=CARTESIAN_POINT('',(-16.261699248248,33.353679903937,207.84762215292));
#25259=CARTESIAN_POINT('',(-13.261699248248,33.3536799039369,207.84762215292));
#25260=CARTESIAN_POINT('',(-16.261699248248,31.653679903937,207.84762215292));
#25261=CARTESIAN_POINT('Origin',(-16.261699248248,31.653679903937,207.84762215292));
#25262=CARTESIAN_POINT('',(-16.261699248248,32.353679903937,203.9));
#25263=CARTESIAN_POINT('',(-16.261699248248,32.353679903937,198.5));
#25264=CARTESIAN_POINT('',(-16.261699248248,33.353679903937,203.9));
#25265=CARTESIAN_POINT('',(-16.261699248248,33.353679903937,207.84762215292));
#25266=CARTESIAN_POINT('',(-16.261699248248,31.653679903937,203.9));
#25267=CARTESIAN_POINT('Origin',(-16.261699248248,31.653679903937,203.9));
#25268=CARTESIAN_POINT('',(-25.061699248248,32.353679903937,203.9));
#25269=CARTESIAN_POINT('',(-69.261699248248,32.353679903937,203.9));
#25270=CARTESIAN_POINT('',(-25.061699248248,33.353679903937,203.9));
#25271=CARTESIAN_POINT('',(-16.261699248248,33.353679903937,203.9));
#25272=CARTESIAN_POINT('',(-25.061699248248,31.653679903937,203.9));
#25273=CARTESIAN_POINT('Origin',(-25.061699248248,31.653679903937,203.9));
#25274=CARTESIAN_POINT('',(-25.061699248248,32.353679903937,201.4));
#25275=CARTESIAN_POINT('',(-25.061699248248,32.353679903937,198.5));
#25276=CARTESIAN_POINT('',(-25.061699248248,33.353679903937,201.4));
#25277=CARTESIAN_POINT('',(-25.061699248248,33.353679903937,203.9));
#25278=CARTESIAN_POINT('',(-25.061699248248,31.653679903937,201.4));
#25279=CARTESIAN_POINT('Origin',(-25.061699248248,31.653679903937,201.4));
#25280=CARTESIAN_POINT('',(-32.261699248248,32.353679903937,201.4));
#25281=CARTESIAN_POINT('',(-69.261699248248,32.353679903937,201.4));
#25282=CARTESIAN_POINT('',(-32.261699248248,33.353679903937,201.4));
#25283=CARTESIAN_POINT('',(-25.061699248248,33.353679903937,201.4));
#25284=CARTESIAN_POINT('',(-32.261699248248,31.653679903937,201.4));
#25285=CARTESIAN_POINT('Origin',(-35.261699248248,31.653679903937,210.957342646887));
#25286=CARTESIAN_POINT('',(-64.261699248248,32.353679903937,210.957342646887));
#25287=CARTESIAN_POINT('',(-35.261699248248,32.353679903937,210.957342646887));
#25288=CARTESIAN_POINT('',(-69.261699248248,32.353679903937,210.957342646887));
#25289=CARTESIAN_POINT('',(-35.261699248248,33.353679903937,210.957342646887));
#25290=CARTESIAN_POINT('',(-35.261699248248,31.653679903937,210.957342646887));
#25291=CARTESIAN_POINT('',(-64.261699248248,33.353679903937,210.957342646887));
#25292=CARTESIAN_POINT('',(-35.261699248248,33.353679903937,210.957342646887));
#25293=CARTESIAN_POINT('',(-64.261699248248,31.653679903937,210.957342646887));
#25294=CARTESIAN_POINT('Origin',(-7.05071200800411,31.6536799039369,207.84762215292));
#25295=CARTESIAN_POINT('',(-7.05071200800411,32.3536799039369,209.34762215292));
#25296=CARTESIAN_POINT('',(-7.05071200800411,32.3536799039369,207.84762215292));
#25297=CARTESIAN_POINT('',(-7.05071200800413,32.3536799039369,198.5));
#25298=CARTESIAN_POINT('',(-7.05071200800411,33.3536799039369,207.84762215292));
#25299=CARTESIAN_POINT('',(-7.05071200800411,31.6536799039369,207.84762215292));
#25300=CARTESIAN_POINT('',(-7.05071200800411,33.3536799039369,209.34762215292));
#25301=CARTESIAN_POINT('',(-7.05071200800411,33.3536799039369,207.84762215292));
#25302=CARTESIAN_POINT('',(-7.05071200800411,31.6536799039369,209.34762215292));
#25303=CARTESIAN_POINT('Origin',(1.43830075175198,31.6536799039369,209.34762215292));
#25304=CARTESIAN_POINT('',(1.43830075175198,32.3536799039369,209.34762215292));
#25305=CARTESIAN_POINT('',(-69.261699248248,32.353679903937,209.34762215292));
#25306=CARTESIAN_POINT('',(1.43830075175198,33.3536799039369,209.34762215292));
#25307=CARTESIAN_POINT('',(1.43830075175198,31.6536799039369,209.34762215292));
#25308=CARTESIAN_POINT('Origin',(1.43830075175198,31.6536799039369,207.84762215292));
#25309=CARTESIAN_POINT('',(1.43830075175198,32.3536799039369,207.84762215292));
#25310=CARTESIAN_POINT('',(-69.261699248248,32.353679903937,207.84762215292));
#25311=CARTESIAN_POINT('',(1.43830075175198,33.3536799039369,207.84762215292));
#25312=CARTESIAN_POINT('',(1.43830075175198,31.6536799039369,207.84762215292));
#25313=CARTESIAN_POINT('',(1.43830075175198,33.3536799039369,207.84762215292));
#25314=CARTESIAN_POINT('Origin',(1.43830075175198,37.6536799039369,207.844898865397));
#25315=CARTESIAN_POINT('',(1.43830075175198,37.6536799039369,207.844898865397));
#25316=CARTESIAN_POINT('',(1.43830075175197,37.6536799039369,198.5));
#25317=CARTESIAN_POINT('Origin',(2.43830075175198,37.6536799039369,207.844898865397));
#25318=CARTESIAN_POINT('',(2.43830075175197,37.6536799039369,198.5));
#25319=CARTESIAN_POINT('',(2.43830075175198,37.6536799039369,207.844898865397));
#25320=CARTESIAN_POINT('Origin',(1.43830075175198,37.6536799039369,207.844898865397));
#25321=CARTESIAN_POINT('',(1.43830075175198,33.3536799039369,207.844898865397));
#25322=CARTESIAN_POINT('',(1.43830075175198,33.3536799039369,207.844898865397));
#25323=CARTESIAN_POINT('',(1.43830075175198,32.3536799039369,207.844898865397));
#25324=CARTESIAN_POINT('',(1.43830075175198,37.6536799039369,207.844898865397));
#25325=CARTESIAN_POINT('',(1.43830075175198,32.3536799039369,207.844898865397));
#25326=CARTESIAN_POINT('Origin',(1.43830075175199,37.6536799039369,209.344898865397));
#25327=CARTESIAN_POINT('',(1.43830075175198,32.3536799039369,209.344898865397));
#25328=CARTESIAN_POINT('',(1.43830075175199,37.6536799039369,209.344898865397));
#25329=CARTESIAN_POINT('',(2.43830075175199,37.6536799039369,209.344898865397));
#25330=CARTESIAN_POINT('',(1.43830075175198,32.3536799039369,209.344898865397));
#25331=CARTESIAN_POINT('Origin',(2.438300751752,37.6536799039369,214.501561642103));
#25332=CARTESIAN_POINT('',(2.438300751752,37.6536799039369,214.501561642103));
#25333=CARTESIAN_POINT('Origin',(1.438300751752,37.6536799039369,214.501561642103));
#25334=CARTESIAN_POINT('',(1.438300751752,32.3536799039369,214.501561642103));
#25335=CARTESIAN_POINT('',(1.438300751752,37.6536799039369,214.501561642103));
#25336=CARTESIAN_POINT('',(1.438300751752,32.3536799039369,214.501561642103));
#25337=CARTESIAN_POINT('Origin',(1.438300751752,37.6536799039369,214.501561642103));
#25338=CARTESIAN_POINT('',(1.43830075175196,32.3536799039369,198.5));
#25339=CARTESIAN_POINT('',(1.438300751752,32.3536799039369,214.5));
#25340=CARTESIAN_POINT('',(1.43830075175199,31.72644166258,214.5));
#25341=CARTESIAN_POINT('',(1.438300751752,32.3536799039369,214.501561642103));
#25342=CARTESIAN_POINT('Origin',(-69.261699248248,33.853679903937,210.465382311583));
#25343=CARTESIAN_POINT('',(-69.261699248248,33.853679903937,209.965382311583));
#25344=CARTESIAN_POINT('',(-69.261699248248,33.353679903937,210.465382311583));
#25345=CARTESIAN_POINT('Origin',(-69.261699248248,33.853679903937,210.465382311583));
#25346=CARTESIAN_POINT('',(-70.261699248248,33.853679903937,209.965382311583));
#25347=CARTESIAN_POINT('',(-68.061699248248,33.853679903937,209.965382311583));
#25348=CARTESIAN_POINT('',(-70.261699248248,33.353679903937,210.465382311583));
#25349=CARTESIAN_POINT('Origin',(-70.261699248248,33.853679903937,210.465382311583));
#25350=CARTESIAN_POINT('',(-69.261699248248,33.353679903937,210.465382311583));
#25351=CARTESIAN_POINT('Origin',(-68.061699248248,33.853679903937,213.325088768032));
#25352=CARTESIAN_POINT('',(-69.261699248248,33.353679903937,213.325088768032));
#25353=CARTESIAN_POINT('',(-69.261699248248,33.853679903937,213.825088768032));
#25354=CARTESIAN_POINT('Origin',(-69.261699248248,33.853679903937,213.325088768032));
#25355=CARTESIAN_POINT('',(-70.261699248248,33.353679903937,213.325088768032));
#25356=CARTESIAN_POINT('',(-69.261699248248,33.353679903937,213.325088768032));
#25357=CARTESIAN_POINT('',(-70.261699248248,33.853679903937,213.825088768032));
#25358=CARTESIAN_POINT('Origin',(-70.261699248248,33.853679903937,213.325088768032));
#25359=CARTESIAN_POINT('',(-68.061699248248,33.853679903937,213.825088768032));
#25360=CARTESIAN_POINT('Origin',(-68.061699248248,34.553679903937,213.325088768032));
#25361=CARTESIAN_POINT('',(-69.261699248248,34.553679903937,213.825088768032));
#25362=CARTESIAN_POINT('Origin',(-69.261699248248,34.553679903937,213.325088768032));
#25363=CARTESIAN_POINT('',(-70.261699248248,34.553679903937,213.825088768032));
#25364=CARTESIAN_POINT('',(-69.261699248248,34.553679903937,213.825088768032));
#25365=CARTESIAN_POINT('Origin',(-70.261699248248,34.553679903937,213.325088768032));
#25366=CARTESIAN_POINT('',(-70.261699248248,35.053679903937,213.325088768032));
#25367=CARTESIAN_POINT('Origin',(-68.061699248248,34.553679903937,210.465382311583));
#25368=CARTESIAN_POINT('',(-69.261699248248,34.553679903937,209.965382311583));
#25369=CARTESIAN_POINT('Origin',(-69.261699248248,34.553679903937,210.465382311583));
#25370=CARTESIAN_POINT('',(-69.261699248248,35.053679903937,210.465382311583));
#25371=CARTESIAN_POINT('',(-70.261699248248,34.553679903937,209.965382311583));
#25372=CARTESIAN_POINT('Origin',(-70.261699248248,34.553679903937,210.465382311583));
#25373=CARTESIAN_POINT('',(-70.261699248248,34.553679903937,209.965382311583));
#25374=CARTESIAN_POINT('Origin',(-69.261699248248,33.353679903937,215.5));
#25375=CARTESIAN_POINT('',(-70.261699248248,33.353679903937,215.5));
#25376=CARTESIAN_POINT('',(-69.261699248248,32.353679903937,198.5));
#25377=CARTESIAN_POINT('',(-70.261699248248,33.353679903937,215.5));
#25378=CARTESIAN_POINT('',(-70.261699248248,33.353679903937,209.965382311583));
#25379=CARTESIAN_POINT('Origin',(-68.061699248248,35.053679903937,213.825088768032));
#25380=CARTESIAN_POINT('',(-70.261699248248,35.053679903937,213.825088768032));
#25381=CARTESIAN_POINT('',(-69.261699248248,35.553679903937,213.825088768032));
#25382=CARTESIAN_POINT('Origin',(-68.061699248248,35.053679903937,209.965382311583));
#25383=CARTESIAN_POINT('Origin',(-68.061699248248,35.053679903937,209.965382311583));
#25384=CARTESIAN_POINT('',(-69.261699248248,35.553679903937,209.965382311583));
#25385=CARTESIAN_POINT('',(-70.261699248248,35.053679903937,209.965382311583));
#25386=CARTESIAN_POINT('Origin',(-69.261699248248,35.553679903937,209.3));
#25387=CARTESIAN_POINT('',(-69.261699248248,33.353679903937,209.3));
#25388=CARTESIAN_POINT('Origin',(-70.261699248248,33.353679903937,215.5));
#25389=CARTESIAN_POINT('Origin',(-70.261699248248,33.353679903937,214.5));
#25390=CARTESIAN_POINT('',(-69.261699248248,33.353679903937,214.5));
#25391=CARTESIAN_POINT('',(-69.261699248248,33.353679903937,214.5));
#25392=CARTESIAN_POINT('',(-69.261699248248,33.353679903937,214.5));
#25393=CARTESIAN_POINT('Origin',(-70.261699248248,33.353679903937,209.3));
#25394=CARTESIAN_POINT('',(-69.261699248248,33.353679903937,209.3));
#25395=CARTESIAN_POINT('',(-69.261699248248,33.353679903937,209.3));
#25396=CARTESIAN_POINT('',(-69.261699248248,33.353679903937,209.3));
#25397=CARTESIAN_POINT('Origin',(-64.261699248248,32.2748332073223,212.5));
#25398=CARTESIAN_POINT('',(-35.261699248248,32.2748332073222,214.210180047071));
#25399=CARTESIAN_POINT('',(-64.261699248248,32.2748332073223,214.210180047071));
#25400=CARTESIAN_POINT('',(-69.261699248248,32.2748332073223,214.210180047071));
#25401=CARTESIAN_POINT('',(-64.261699248248,32.2748332073223,215.5));
#25402=CARTESIAN_POINT('',(-64.261699248248,32.2748332073223,212.5));
#25403=CARTESIAN_POINT('',(-35.261699248248,32.2748332073222,215.5));
#25404=CARTESIAN_POINT('',(-64.261699248248,32.2748332073223,215.5));
#25405=CARTESIAN_POINT('',(-35.261699248248,32.2748332073222,212.5));
#25406=CARTESIAN_POINT('Origin',(-35.261699248248,33.7748332073222,212.5));
#25407=CARTESIAN_POINT('',(-35.261699248248,33.353679903937,214.5));
#25408=CARTESIAN_POINT('Origin',(-35.261699248248,31.72644166258,213.826414496105));
#25409=CARTESIAN_POINT('',(-35.261699248248,33.353679903937,214.5));
#25410=CARTESIAN_POINT('',(-35.261699248248,32.353679903937,214.095949172));
#25411=CARTESIAN_POINT('',(-35.261699248248,32.353679903937,198.5));
#25412=CARTESIAN_POINT('Origin',(-35.261699248248,30.5438127434663,212.93103382282));
#25413=CARTESIAN_POINT('Origin',(-64.261699248248,33.7748332073223,212.5));
#25414=CARTESIAN_POINT('Origin',(-64.261699248248,30.5438127434664,212.93103382282));
#25415=CARTESIAN_POINT('',(-64.261699248248,32.353679903937,198.5));
#25416=CARTESIAN_POINT('',(-64.261699248248,33.353679903937,214.5));
#25417=CARTESIAN_POINT('',(-64.261699248248,33.353679903937,214.5));
#25418=CARTESIAN_POINT('Origin',(-64.261699248248,31.72644166258,213.826414496105));
#25419=CARTESIAN_POINT('Origin',(-32.261699248248,32.2748332073222,212.5));
#25420=CARTESIAN_POINT('',(-16.261699248248,32.2748332073222,214.210180047071));
#25421=CARTESIAN_POINT('',(-32.261699248248,32.2748332073222,214.210180047071));
#25422=CARTESIAN_POINT('',(-69.261699248248,32.2748332073223,214.210180047071));
#25423=CARTESIAN_POINT('',(-32.261699248248,32.2748332073222,215.5));
#25424=CARTESIAN_POINT('',(-32.261699248248,32.2748332073222,212.5));
#25425=CARTESIAN_POINT('',(-16.261699248248,32.2748332073222,215.5));
#25426=CARTESIAN_POINT('',(-32.261699248248,32.2748332073222,215.5));
#25427=CARTESIAN_POINT('',(-16.261699248248,32.2748332073222,212.5));
#25428=CARTESIAN_POINT('Origin',(-16.261699248248,32.2748332073222,212.5));
#25429=CARTESIAN_POINT('',(-16.261699248248,33.353679903937,214.5));
#25430=CARTESIAN_POINT('Origin',(-16.261699248248,31.72644166258,213.826414496105));
#25431=CARTESIAN_POINT('',(-16.261699248248,33.353679903937,214.5));
#25432=CARTESIAN_POINT('',(-16.261699248248,32.353679903937,214.095949172));
#25433=CARTESIAN_POINT('',(-16.261699248248,32.353679903937,198.5));
#25434=CARTESIAN_POINT('Origin',(-16.261699248248,30.5438127434663,212.93103382282));
#25435=CARTESIAN_POINT('Origin',(-32.261699248248,32.2748332073222,212.5));
#25436=CARTESIAN_POINT('',(-32.261699248248,32.353679903937,214.095949172));
#25437=CARTESIAN_POINT('',(-32.261699248248,32.353679903937,214.471369141518));
#25438=CARTESIAN_POINT('',(-32.261699248248,33.353679903937,214.5));
#25439=CARTESIAN_POINT('',(-32.261699248248,33.353679903937,214.5));
#25440=CARTESIAN_POINT('Origin',(-32.261699248248,31.72644166258,213.826414496105));
#25441=CARTESIAN_POINT('Origin',(-32.261699248248,30.5438127434663,212.93103382282));
#25442=CARTESIAN_POINT('Origin',(-65.261699248248,27.1079166291735,201.645652141467));
#25443=CARTESIAN_POINT('',(-66.861699248248,27.1079166291735,214.5));
#25444=CARTESIAN_POINT('',(-66.861699248248,27.1079166291735,215.5));
#25445=CARTESIAN_POINT('',(-66.861699248248,27.1079166291735,201.645652141467));
#25446=CARTESIAN_POINT('',(-63.661699248248,27.1079166291735,215.5));
#25447=CARTESIAN_POINT('Origin',(-65.261699248248,27.1079166291735,215.5));
#25448=CARTESIAN_POINT('',(-63.661699248248,27.1079166291735,214.5));
#25449=CARTESIAN_POINT('',(-63.661699248248,27.1079166291735,201.645652141467));
#25450=CARTESIAN_POINT('Origin',(-65.261699248248,27.1079166291735,214.5));
#25451=CARTESIAN_POINT('Origin',(-66.861699248248,27.1079166291735,201.645652141467));
#25452=CARTESIAN_POINT('',(-66.861699248248,29.6079166291735,214.5));
#25453=CARTESIAN_POINT('',(-66.861699248248,29.6079166291735,215.5));
#25454=CARTESIAN_POINT('',(-66.861699248248,29.6079166291735,201.645652141467));
#25455=CARTESIAN_POINT('',(-66.861699248248,27.1079166291735,215.5));
#25456=CARTESIAN_POINT('',(-66.861699248248,27.1079166291735,214.5));
#25457=CARTESIAN_POINT('Origin',(-65.261699248248,29.6079166291735,201.645652141467));
#25458=CARTESIAN_POINT('',(-63.661699248248,29.6079166291735,214.5));
#25459=CARTESIAN_POINT('',(-63.661699248248,29.6079166291735,215.5));
#25460=CARTESIAN_POINT('',(-63.661699248248,29.6079166291735,201.645652141467));
#25461=CARTESIAN_POINT('Origin',(-65.261699248248,29.6079166291735,215.5));
#25462=CARTESIAN_POINT('Origin',(-65.261699248248,29.6079166291735,214.5));
#25463=CARTESIAN_POINT('Origin',(-63.661699248248,27.1079166291735,201.645652141467));
#25464=CARTESIAN_POINT('',(-63.661699248248,27.1079166291735,215.5));
#25465=CARTESIAN_POINT('',(-63.661699248248,27.1079166291735,214.5));
#25466=CARTESIAN_POINT('Origin',(-11.261699248248,27.1079166291735,201.645652141467));
#25467=CARTESIAN_POINT('',(-12.861699248248,27.1079166291735,214.5));
#25468=CARTESIAN_POINT('',(-12.861699248248,27.1079166291735,215.5));
#25469=CARTESIAN_POINT('',(-12.861699248248,27.1079166291735,201.645652141467));
#25470=CARTESIAN_POINT('',(-9.66169924824801,27.1079166291735,215.5));
#25471=CARTESIAN_POINT('Origin',(-11.261699248248,27.1079166291735,215.5));
#25472=CARTESIAN_POINT('',(-9.66169924824801,27.1079166291735,214.5));
#25473=CARTESIAN_POINT('',(-9.66169924824804,27.1079166291735,201.645652141467));
#25474=CARTESIAN_POINT('Origin',(-11.261699248248,27.1079166291735,214.5));
#25475=CARTESIAN_POINT('Origin',(-12.861699248248,27.1079166291735,201.645652141467));
#25476=CARTESIAN_POINT('',(-12.861699248248,29.6079166291735,214.5));
#25477=CARTESIAN_POINT('',(-12.861699248248,29.6079166291735,215.5));
#25478=CARTESIAN_POINT('',(-12.861699248248,29.6079166291735,201.645652141467));
#25479=CARTESIAN_POINT('',(-12.861699248248,27.1079166291735,215.5));
#25480=CARTESIAN_POINT('',(-12.861699248248,27.1079166291735,214.5));
#25481=CARTESIAN_POINT('Origin',(-11.261699248248,29.6079166291735,201.645652141467));
#25482=CARTESIAN_POINT('',(-9.66169924824801,29.6079166291735,214.5));
#25483=CARTESIAN_POINT('',(-9.66169924824801,29.6079166291735,215.5));
#25484=CARTESIAN_POINT('',(-9.66169924824804,29.6079166291735,201.645652141467));
#25485=CARTESIAN_POINT('Origin',(-11.261699248248,29.6079166291735,215.5));
#25486=CARTESIAN_POINT('Origin',(-11.261699248248,29.6079166291735,214.5));
#25487=CARTESIAN_POINT('Origin',(-9.66169924824804,27.1079166291735,201.645652141467));
#25488=CARTESIAN_POINT('',(-9.66169924824801,27.1079166291735,215.5));
#25489=CARTESIAN_POINT('',(-9.66169924824801,27.1079166291735,214.5));
#25490=CARTESIAN_POINT('Origin',(-7.26169924824804,24.053679903937,201.645652141467));
#25491=CARTESIAN_POINT('',(-7.261699248248,33.3536799039369,214.5));
#25492=CARTESIAN_POINT('',(-7.261699248248,32.2748332073222,215.5));
#25493=CARTESIAN_POINT('Origin',(-7.26169924824801,31.72644166258,213.826414496105));
#25494=CARTESIAN_POINT('',(-7.26169924824801,24.053679903937,215.5));
#25495=CARTESIAN_POINT('',(-7.26169924824801,24.053679903937,215.5));
#25496=CARTESIAN_POINT('',(-7.26169924824802,24.053679903937,214.5));
#25497=CARTESIAN_POINT('',(-7.26169924824804,24.053679903937,201.645652141467));
#25498=CARTESIAN_POINT('',(-7.261699248248,32.0172414129883,214.5));
#25499=CARTESIAN_POINT('',(-7.26169924824802,24.053679903937,214.5));
#25500=CARTESIAN_POINT('',(-7.26169924824802,24.053679903937,214.5));
#25501=CARTESIAN_POINT('Origin',(-69.261699248248,32.0172414129883,214.5));
#25502=CARTESIAN_POINT('',(-69.261699248248,33.353679903937,214.5));
#25503=CARTESIAN_POINT('',(1.438300751752,32.0172414129883,214.5));
#25504=CARTESIAN_POINT('',(-69.261699248248,32.0172414129883,214.5));
#25505=CARTESIAN_POINT('',(1.43830075175199,31.72644166258,214.5));
#25506=CARTESIAN_POINT('Origin',(1.43830075175199,31.72644166258,213.826414496105));
#25507=CARTESIAN_POINT('',(1.43830075175199,32.3536799039369,214.095949171999));
#25508=CARTESIAN_POINT('',(1.438300751752,32.3536799039369,214.501561642103));
#25509=CARTESIAN_POINT('Origin',(1.43830075175199,30.5438127434663,212.93103382282));
#25510=CARTESIAN_POINT('Origin',(-69.261699248248,32.0172414129883,214.5));
#25511=CARTESIAN_POINT('',(-69.261699248248,24.053679903937,214.5));
#25512=CARTESIAN_POINT('',(-69.261699248248,24.053679903937,214.5));
#25513=CARTESIAN_POINT('',(-69.261699248248,32.0172414129883,214.5));
#25514=CARTESIAN_POINT('',(-69.261699248248,32.0172414129883,214.5));
#25515=CARTESIAN_POINT('',(-69.261699248248,32.0172414129883,214.5));
#25516=CARTESIAN_POINT('Origin',(-69.261699248248,30.5438127434664,212.93103382282));
#25517=CARTESIAN_POINT('',(-69.261699248248,32.353679903937,214.095949172));
#25518=CARTESIAN_POINT('',(-69.261699248248,32.353679903937,214.095949172));
#25519=CARTESIAN_POINT('Origin',(-69.261699248248,30.5438127434664,212.93103382282));
#25520=CARTESIAN_POINT('Origin',(-69.261699248248,32.353679903937,198.5));
#25521=CARTESIAN_POINT('',(-69.261699248248,32.353679903937,198.5));
#25522=CARTESIAN_POINT('',(-69.261699248248,32.353679903937,198.5));
#25523=CARTESIAN_POINT('',(-69.261699248248,32.353679903937,198.5));
#25524=CARTESIAN_POINT('',(1.43830075175196,32.3536799039369,198.5));
#25525=CARTESIAN_POINT('',(-32.261699248248,32.353679903937,198.5));
#25526=CARTESIAN_POINT('Origin',(-69.261699248248,33.353679903937,198.5));
#25527=CARTESIAN_POINT('',(-69.261699248248,33.353679903937,198.5));
#25528=CARTESIAN_POINT('',(-69.261699248248,33.353679903937,198.5));
#25529=CARTESIAN_POINT('',(-69.261699248248,33.353679903937,198.5));
#25530=CARTESIAN_POINT('Origin',(-69.261699248248,33.353679903937,214.5));
#25531=CARTESIAN_POINT('',(-32.261699248248,33.353679903937,214.5));
#25532=CARTESIAN_POINT('',(-69.261699248248,33.353679903937,214.5));
#25533=CARTESIAN_POINT('',(1.438300751752,33.3536799039369,214.5));
#25534=CARTESIAN_POINT('',(-69.261699248248,33.353679903937,214.5));
#25535=CARTESIAN_POINT('',(-69.261699248248,33.353679903937,209.3));
#25536=CARTESIAN_POINT('',(-69.261699248248,33.353679903937,214.5));
#25537=CARTESIAN_POINT('',(-69.261699248248,33.353679903937,214.5));
#25538=CARTESIAN_POINT('Origin',(-69.261699248248,31.72644166258,213.826414496105));
#25539=CARTESIAN_POINT('',(-69.261699248248,32.2748332073223,215.5));
#25540=CARTESIAN_POINT('Origin',(-69.261699248248,24.053679903937,215.5));
#25541=CARTESIAN_POINT('',(-69.261699248248,32.2748332073223,215.5));
#25542=CARTESIAN_POINT('',(-69.261699248248,32.2748332073223,215.5));
#25543=CARTESIAN_POINT('',(-69.261699248248,32.2748332073223,215.5));
#25544=CARTESIAN_POINT('',(-69.261699248248,24.053679903937,215.5));
#25545=CARTESIAN_POINT('',(-69.261699248248,24.053679903937,215.5));
#25546=CARTESIAN_POINT('',(-69.261699248248,24.053679903937,215.5));
#25547=CARTESIAN_POINT('Origin',(-69.261699248248,24.053679903937,214.5));
#25548=CARTESIAN_POINT('',(-69.261699248248,24.053679903937,214.5));
#25549=CARTESIAN_POINT('Origin',(-69.261699248248,31.72644166258,213.826414496105));
#25550=CARTESIAN_POINT('Origin',(-69.261699248248,31.72644166258,213.826414496105));
#25551=CARTESIAN_POINT('Origin',(-69.261699248248,31.72644166258,213.826414496105));
#25552=CARTESIAN_POINT('Origin',(-69.261699248248,31.72644166258,213.826414496105));
#25553=CARTESIAN_POINT('Origin',(-69.261699248248,31.72644166258,213.826414496105));
#25554=CARTESIAN_POINT('Origin',(1.43830075175199,31.72644166258,213.826414496105));
#25555=CARTESIAN_POINT('Origin',(-32.261699248248,32.2748332073222,212.5));
#25556=CARTESIAN_POINT('Origin',(-70.261699248248,33.353679903937,215.5));
#25557=CARTESIAN_POINT('Origin',(-69.261699248248,35.553679903937,209.3));
#25558=CARTESIAN_POINT('',(0.,0.,0.));
#25559=CARTESIAN_POINT('Origin',(77.9152339218055,61.1315783931225,207.276481344607));
#25560=CARTESIAN_POINT('',(78.1645204353182,61.1504525601425,207.276481344607));
#25561=CARTESIAN_POINT('',(77.9152339218055,61.1315783931225,207.526481344607));
#25562=CARTESIAN_POINT('Origin',(77.9152339218055,61.1315783931226,207.276481344607));
#25563=CARTESIAN_POINT('',(77.9243166636283,60.8817434400015,207.276481344607));
#25564=CARTESIAN_POINT('Origin',(77.9152339218055,61.1315783931225,207.276481344607));
#25565=CARTESIAN_POINT('Origin',(77.9152339218055,61.1315783931226,207.276481344607));
#25566=CARTESIAN_POINT('Origin',(59.7044966368782,72.3742118764312,207.276481344607));
#25567=CARTESIAN_POINT('',(59.4770762970785,72.2703851503661,207.276481344607));
#25568=CARTESIAN_POINT('',(59.6095124682004,72.6054650011681,207.276481344607));
#25569=CARTESIAN_POINT('Origin',(59.7044966368782,72.3742118764312,207.276481344607));
#25570=CARTESIAN_POINT('',(59.7044966368782,72.3742118764312,207.526481344607));
#25571=CARTESIAN_POINT('Origin',(59.7044966368782,72.3742118764312,207.276481344607));
#25572=CARTESIAN_POINT('Origin',(59.7044966368782,72.3742118764312,207.276481344607));
#25573=CARTESIAN_POINT('Origin',(79.3271639989382,62.3514930904775,207.276481344607));
#25574=CARTESIAN_POINT('',(79.2329453452574,62.5828815339371,207.285549615221));
#25575=CARTESIAN_POINT('',(79.0778774854255,62.3326189234576,207.276481344607));
#25576=CARTESIAN_POINT('Origin',(79.3271639989382,62.3514930904775,207.276481344607));
#25577=CARTESIAN_POINT('',(79.3271639989382,62.3514930904775,207.526481344607));
#25578=CARTESIAN_POINT('Origin',(79.3271639989382,62.3514930904775,207.276481344607));
#25579=CARTESIAN_POINT('',(79.2991550620136,62.5905151532426,207.3441862409));
#25580=CARTESIAN_POINT('Origin',(79.3271639989382,62.3514930904775,207.276481344607));
#25581=CARTESIAN_POINT('Ctrl Pts',(79.2991550620136,62.5905151532426,207.344186240766));
#25582=CARTESIAN_POINT('Ctrl Pts',(79.2936414483863,62.5898690603484,207.344186240766));
#25583=CARTESIAN_POINT('Ctrl Pts',(79.2876554089815,62.5891704418728,207.343449242348));
#25584=CARTESIAN_POINT('Ctrl Pts',(79.2761242753789,62.5878305349169,207.340322634924));
#25585=CARTESIAN_POINT('Ctrl Pts',(79.2705791816217,62.5871892200478,207.337933035602));
#25586=CARTESIAN_POINT('Ctrl Pts',(79.260853293221,62.5860680140522,207.332255389429));
#25587=CARTESIAN_POINT('Ctrl Pts',(79.2561763647588,62.5855310114079,207.328654585832));
#25588=CARTESIAN_POINT('Ctrl Pts',(79.2478683053229,62.5845797700644,207.320274409274));
#25589=CARTESIAN_POINT('Ctrl Pts',(79.2442358923008,62.5841654166262,207.315496320451));
#25590=CARTESIAN_POINT('Ctrl Pts',(79.2369361747333,62.5833339506126,207.302683579489));
#25591=CARTESIAN_POINT('Ctrl Pts',(79.2340922950462,62.5830116078114,207.294147337792));
#25592=CARTESIAN_POINT('Ctrl Pts',(79.232945345238,62.582881533935,207.285549615073));
#25593=CARTESIAN_POINT('Origin',(95.7290969072821,75.0941505546249,207.276481344607));
#25594=CARTESIAN_POINT('',(95.788180276892,75.3370685560895,207.276481344607));
#25595=CARTESIAN_POINT('',(95.7290969072821,75.0941505546249,207.526481344607));
#25596=CARTESIAN_POINT('Origin',(95.7290969072821,75.0941505546249,207.276481344607));
#25597=CARTESIAN_POINT('',(95.969528519046,75.0256477074975,207.276481344607));
#25598=CARTESIAN_POINT('Origin',(95.7290969072821,75.0941505546249,207.276481344607));
#25599=CARTESIAN_POINT('Origin',(95.7290969072821,75.0941505546249,207.276481344607));
#25600=CARTESIAN_POINT('Origin',(60.1621734217283,74.1837962848936,207.276481344607));
#25601=CARTESIAN_POINT('',(60.1621734217283,74.1837962848936,207.526481344607));
#25602=CARTESIAN_POINT('',(60.3884110190581,74.2658486863688,207.344186240786));
#25603=CARTESIAN_POINT('Origin',(60.1621734217283,74.1837962848936,207.276481344607));
#25604=CARTESIAN_POINT('',(60.2571575904061,73.9525431601567,207.276481344607));
#25605=CARTESIAN_POINT('Origin',(60.1621734217283,74.1837962848936,207.276481344607));
#25606=CARTESIAN_POINT('',(60.4112511369769,74.2032374366335,207.285547783929));
#25607=CARTESIAN_POINT('Origin',(60.1621734217283,74.1837962848936,207.276481344607));
#25608=CARTESIAN_POINT('Ctrl Pts',(60.4112515042303,74.2032360650638,207.285547973752));
#25609=CARTESIAN_POINT('Ctrl Pts',(60.4108539539671,74.2043195996929,207.294146250025));
#25610=CARTESIAN_POINT('Ctrl Pts',(60.4098679175592,74.2070065582381,207.302683093175));
#25611=CARTESIAN_POINT('Ctrl Pts',(60.407340557639,74.2139053814473,207.315496320451));
#25612=CARTESIAN_POINT('Ctrl Pts',(60.4060835087816,74.2173384473227,207.320274409274));
#25613=CARTESIAN_POINT('Ctrl Pts',(60.4032115424655,74.2251921420687,207.328654585832));
#25614=CARTESIAN_POINT('Ctrl Pts',(60.4015961531691,74.2296139685129,207.332255389429));
#25615=CARTESIAN_POINT('Ctrl Pts',(60.3982408855922,74.2388113696434,207.337933035602));
#25616=CARTESIAN_POINT('Ctrl Pts',(60.3963297752376,74.2440560819091,207.340322634924));
#25617=CARTESIAN_POINT('Ctrl Pts',(60.3923611971915,74.254965379829,207.343449242348));
#25618=CARTESIAN_POINT('Ctrl Pts',(60.3903037532893,74.2606299769125,207.344186240766));
#25619=CARTESIAN_POINT('Ctrl Pts',(60.3884110190634,74.2658486863707,207.344186240766));
#25620=CARTESIAN_POINT('Origin',(96.0835971249419,76.5516585634122,207.276481344607));
#25621=CARTESIAN_POINT('',(96.0835971249419,76.5516585634122,207.526481344607));
#25622=CARTESIAN_POINT('',(96.3286326356366,76.5020843917236,207.276481344607));
#25623=CARTESIAN_POINT('Origin',(96.0835971249419,76.5516585634122,207.276481344607));
#25624=CARTESIAN_POINT('',(96.0245137553319,76.3087405619477,207.276481344607));
#25625=CARTESIAN_POINT('Origin',(96.0835971249419,76.5516585634122,207.276481344607));
#25626=CARTESIAN_POINT('Origin',(96.0835971249419,76.5516585634122,207.276481344607));
#25627=CARTESIAN_POINT('Origin',(64.9174359473229,93.7042420150737,207.276481344607));
#25628=CARTESIAN_POINT('',(65.1080190161996,93.8660384731857,207.276481344607));
#25629=CARTESIAN_POINT('',(64.9174359473229,93.7042420150737,207.526481344607));
#25630=CARTESIAN_POINT('Origin',(64.9174359473229,93.7042420150737,207.276481344607));
#25631=CARTESIAN_POINT('',(65.0805892967552,93.5273323443229,207.344186240766));
#25632=CARTESIAN_POINT('Origin',(64.9174359473229,93.7042420150737,207.276481344607));
#25633=CARTESIAN_POINT('',(65.1296671539667,93.5724251671486,207.285549615094));
#25634=CARTESIAN_POINT('Ctrl Pts',(65.0805892967552,93.5273323443229,207.344186240766));
#25635=CARTESIAN_POINT('Ctrl Pts',(65.0846701400053,93.5310958652313,207.344186240766));
#25636=CARTESIAN_POINT('Ctrl Pts',(65.0891023099758,93.5351795651324,207.343449242348));
#25637=CARTESIAN_POINT('Ctrl Pts',(65.0976436154766,93.5430414029044,207.340322634924));
#25638=CARTESIAN_POINT('Ctrl Pts',(65.1017527351394,93.5468195618653,207.337933035602));
#25639=CARTESIAN_POINT('Ctrl Pts',(65.108962115792,93.5534433703373,207.332255389428));
#25640=CARTESIAN_POINT('Ctrl Pts',(65.1124301881646,93.5566268441787,207.328654585832));
#25641=CARTESIAN_POINT('Ctrl Pts',(65.1185924238054,93.5622797694029,207.320274409274));
#25642=CARTESIAN_POINT('Ctrl Pts',(65.1212875568307,93.5647500671807,207.315496320451));
#25643=CARTESIAN_POINT('Ctrl Pts',(65.1267044289337,93.5697134036456,207.302683579495));
#25644=CARTESIAN_POINT('Ctrl Pts',(65.128815707585,93.5716457749885,207.294147337805));
#25645=CARTESIAN_POINT('Ctrl Pts',(65.1296671539667,93.5724251671486,207.285549615094));
#25646=CARTESIAN_POINT('Origin',(64.9174359473229,93.7042420150737,207.276481344607));
#25647=CARTESIAN_POINT('Origin',(87.370415498102,95.4011189555928,207.276481344607));
#25648=CARTESIAN_POINT('',(87.1804067618325,95.2389020358428,207.285548914041));
#25649=CARTESIAN_POINT('',(87.1576445151781,95.5323763699572,207.276481344607));
#25650=CARTESIAN_POINT('Origin',(87.370415498102,95.4011189555928,207.276481344607));
#25651=CARTESIAN_POINT('',(87.235703204888,95.2016981816169,207.344186240766));
#25652=CARTESIAN_POINT('Ctrl Pts',(87.1804056812849,95.2389029103722,207.285549099905));
#25653=CARTESIAN_POINT('Ctrl Pts',(87.1813645562961,95.2382603596069,207.294146996371));
#25654=CARTESIAN_POINT('Ctrl Pts',(87.1837422934887,95.2366672287293,207.302683426847));
#25655=CARTESIAN_POINT('Ctrl Pts',(87.1898436571226,95.2325743250902,207.315496320451));
#25656=CARTESIAN_POINT('Ctrl Pts',(87.1928794417903,95.2305371396332,207.320274409274));
#25657=CARTESIAN_POINT('Ctrl Pts',(87.1998212692631,95.2258745498999,207.328654585832));
#25658=CARTESIAN_POINT('Ctrl Pts',(87.2037283980161,95.2232484545878,207.332255389428));
#25659=CARTESIAN_POINT('Ctrl Pts',(87.211851391824,95.2177833855431,207.337933035602));
#25660=CARTESIAN_POINT('Ctrl Pts',(87.2164816625401,95.2146657032897,207.340322634924));
#25661=CARTESIAN_POINT('Ctrl Pts',(87.2261075175784,95.2081768430205,207.343449242348));
#25662=CARTESIAN_POINT('Ctrl Pts',(87.231103089383,95.2048056417694,207.344186240766));
#25663=CARTESIAN_POINT('Ctrl Pts',(87.235703204888,95.2016981816168,207.344186240766));
#25664=CARTESIAN_POINT('',(87.370415498102,95.4011189555928,207.526481344607));
#25665=CARTESIAN_POINT('Origin',(87.370415498102,95.4011189555928,207.276481344607));
#25666=CARTESIAN_POINT('Origin',(87.370415498102,95.4011189555928,207.276481344607));
#25667=CARTESIAN_POINT('Origin',(65.3426635064322,95.5210854135286,207.276481344607));
#25668=CARTESIAN_POINT('',(65.1884661129904,95.7178674346986,207.276481344607));
#25669=CARTESIAN_POINT('',(65.1520804375556,95.3592889554166,207.276481344607));
#25670=CARTESIAN_POINT('Origin',(65.3426635064322,95.5210854135286,207.276481344607));
#25671=CARTESIAN_POINT('',(65.3426635064322,95.5210854135286,207.526481344607));
#25672=CARTESIAN_POINT('Origin',(65.3426635064322,95.5210854135286,207.276481344607));
#25673=CARTESIAN_POINT('Origin',(65.3426635064322,95.5210854135286,207.276481344607));
#25674=CARTESIAN_POINT('Origin',(86.6766969576459,97.1335683214121,207.276481344607));
#25675=CARTESIAN_POINT('',(86.7995649337003,97.3512916790481,207.276481344607));
#25676=CARTESIAN_POINT('',(86.6766969576459,97.1335683214121,207.526481344607));
#25677=CARTESIAN_POINT('Origin',(86.6766969576459,97.1335683214121,207.276481344607));
#25678=CARTESIAN_POINT('',(86.8894679405697,97.0023109070477,207.276481344607));
#25679=CARTESIAN_POINT('Origin',(86.6766969576459,97.1335683214121,207.276481344607));
#25680=CARTESIAN_POINT('Origin',(86.6766969576459,97.1335683214121,207.276481344607));
#25681=CARTESIAN_POINT('Origin',(77.215862801455,80.368869783441,207.2));
#25682=CARTESIAN_POINT('',(82.4344268912437,95.2821721957428,207.2));
#25683=CARTESIAN_POINT('Origin',(77.215862801455,80.368869783441,207.2));
#25684=CARTESIAN_POINT('',(82.335340231311,94.999008225889,207.5));
#25685=CARTESIAN_POINT('Origin',(82.335340231311,94.999008225889,207.2));
#25686=CARTESIAN_POINT('Origin',(77.215862801455,80.368869783441,207.5));
#25687=CARTESIAN_POINT('Origin',(77.215862801455,80.368869783441,209.104699448314));
#25688=CARTESIAN_POINT('',(87.6199620943882,110.101086618093,209.104699448314));
#25689=CARTESIAN_POINT('',(66.8117635085218,50.6366529487886,209.104699448314));
#25690=CARTESIAN_POINT('Origin',(77.215862801455,80.368869783441,209.104699448314));
#25691=CARTESIAN_POINT('Origin',(77.215862801455,80.368869783441,209.104699448314));
#25692=CARTESIAN_POINT('',(66.9092858372326,50.9153464658161,209.404662059183));
#25693=CARTESIAN_POINT('Origin',(66.9108501684545,50.9198169186424,209.104699448314));
#25694=CARTESIAN_POINT('Origin',(77.215862801455,80.368869783441,209.404662059183));
#25695=CARTESIAN_POINT('Origin',(77.215862801455,80.368869783441,209.995300551686));
#25696=CARTESIAN_POINT('',(81.344473631984,92.1673685273507,209.995300551686));
#25697=CARTESIAN_POINT('Origin',(77.215862801455,80.368869783441,209.995300551686));
#25698=CARTESIAN_POINT('',(81.4419959606949,92.4460620443781,209.695337940817));
#25699=CARTESIAN_POINT('Origin',(81.4435602919167,92.4505324972045,209.995300551686));
#25700=CARTESIAN_POINT('',(72.9897296422151,68.2916775225039,209.695337940817));
#25701=CARTESIAN_POINT('Origin',(77.215862801455,80.368869783441,209.695337940817));
#25702=CARTESIAN_POINT('Origin',(77.215862801455,80.368869783441,209.695337940817));
#25703=CARTESIAN_POINT('Origin',(77.215862801455,80.368869783441,207.8));
#25704=CARTESIAN_POINT('',(80.6838958990994,90.2796087283251,207.5));
#25705=CARTESIAN_POINT('Origin',(77.215862801455,80.368869783441,207.5));
#25706=CARTESIAN_POINT('',(80.5848092391667,89.9964447584713,207.8));
#25707=CARTESIAN_POINT('Origin',(80.6838958990994,90.2796087283251,207.8));
#25708=CARTESIAN_POINT('Origin',(77.215862801455,80.368869783441,207.8));
#25709=CARTESIAN_POINT('Origin',(77.215862801455,80.368869783441,209.7));
#25710=CARTESIAN_POINT('',(73.7478297038106,70.4581308385569,210.));
#25711=CARTESIAN_POINT('Origin',(77.215862801455,80.368869783441,210.));
#25712=CARTESIAN_POINT('',(73.8469163637433,70.7412948084107,209.7));
#25713=CARTESIAN_POINT('Origin',(73.7478297038106,70.4581308385569,209.7));
#25714=CARTESIAN_POINT('',(80.5848092391667,89.9964447584713,209.7));
#25715=CARTESIAN_POINT('Origin',(77.215862801455,80.368869783441,209.7));
#25716=CARTESIAN_POINT('Origin',(77.215862801455,80.368869783441,209.7));
#25717=CARTESIAN_POINT('Origin',(77.215862801455,80.368869783441,208.4));
#25718=CARTESIAN_POINT('',(87.6199620943882,110.101086618093,208.4));
#25719=CARTESIAN_POINT('Origin',(77.215862801455,80.368869783441,208.4));
#25720=CARTESIAN_POINT('',(87.5208754344555,109.81792264824,208.1));
#25721=CARTESIAN_POINT('Origin',(87.5208754344555,109.81792264824,208.4));
#25722=CARTESIAN_POINT('Origin',(77.215862801455,80.368869783441,208.1));
#25723=CARTESIAN_POINT('Origin',(77.215862801455,80.368869783441,207.8));
#25724=CARTESIAN_POINT('',(83.2271201707053,97.5474839545735,208.1));
#25725=CARTESIAN_POINT('Origin',(77.215862801455,80.368869783441,208.1));
#25726=CARTESIAN_POINT('',(83.1280335107726,97.2643199847197,207.8));
#25727=CARTESIAN_POINT('Origin',(83.2271201707053,97.5474839545735,207.8));
#25728=CARTESIAN_POINT('Origin',(77.215862801455,80.368869783441,207.8));
#25729=CARTESIAN_POINT('Origin',(77.215862801455,80.368869783441,198.));
#25730=CARTESIAN_POINT('',(83.000126282037,96.8987943056185,197.986679815914));
#25731=CARTESIAN_POINT('Origin',(77.215862801455,80.368869783441,197.986679815914));
#25732=CARTESIAN_POINT('',(82.9011373407276,96.6159095902407,197.7));
#25733=CARTESIAN_POINT('Origin',(82.9011373407276,96.6159095902407,198.));
#25734=CARTESIAN_POINT('Origin',(77.215862801455,80.368869783441,197.7));
#25735=CARTESIAN_POINT('Origin',(77.215862801455,80.368869783441,198.));
#25736=CARTESIAN_POINT('',(82.5335135511764,95.5653361655966,197.7));
#25737=CARTESIAN_POINT('Origin',(77.215862801455,80.368869783441,197.7));
#25738=CARTESIAN_POINT('',(82.4344268912437,95.2821721957428,198.));
#25739=CARTESIAN_POINT('Origin',(82.5335135511764,95.5653361655966,198.));
#25740=CARTESIAN_POINT('Origin',(77.215862801455,80.368869783441,198.));
#25741=CARTESIAN_POINT('Origin',(77.215862801455,80.368869783441,209.7));
#25742=CARTESIAN_POINT('',(87.6199620943882,110.101086618093,209.7));
#25743=CARTESIAN_POINT('Origin',(77.215862801455,80.368869783441,209.7));
#25744=CARTESIAN_POINT('',(83.1280335107726,97.2643199847197,207.344186240766));
#25745=CARTESIAN_POINT('',(83.1280335107726,97.2643199847197,209.7));
#25746=CARTESIAN_POINT('',(66.2091808261905,94.4849227691515,207.344186240766));
#25747=CARTESIAN_POINT('Origin',(77.215862801455,80.368869783441,207.344186240766));
#25748=CARTESIAN_POINT('',(66.156698979235,94.4438437095257,207.285548215601));
#25749=CARTESIAN_POINT('Ctrl Pts',(66.156697797991,94.4438429424263,207.285548403906));
#25750=CARTESIAN_POINT('Ctrl Pts',(66.157605358421,94.4445560422264,207.294146535105));
#25751=CARTESIAN_POINT('Ctrl Pts',(66.1598557893509,94.4463245033558,207.302683220627));
#25752=CARTESIAN_POINT('Ctrl Pts',(66.1656351357801,94.4508609547001,207.315496320451));
#25753=CARTESIAN_POINT('Ctrl Pts',(66.1685113430769,94.4531178429828,207.320274409274));
#25754=CARTESIAN_POINT('Ctrl Pts',(66.1750922888656,94.4582772871593,207.328654585832));
#25755=CARTESIAN_POINT('Ctrl Pts',(66.1787980203727,94.4611806620366,207.332255389429));
#25756=CARTESIAN_POINT('Ctrl Pts',(66.1865074101033,94.4672151726256,207.337933035602));
#25757=CARTESIAN_POINT('Ctrl Pts',(66.1909042788197,94.4706541979277,207.340322634924));
#25758=CARTESIAN_POINT('Ctrl Pts',(66.2000520670299,94.4778012507239,207.343449242348));
#25759=CARTESIAN_POINT('Ctrl Pts',(66.2048030047484,94.4815092591281,207.344186240766));
#25760=CARTESIAN_POINT('Ctrl Pts',(66.2091808261905,94.4849227691515,207.344186240766));
#25761=CARTESIAN_POINT('',(66.1149823135236,94.4109655092461,206.699999966761));
#25762=CARTESIAN_POINT('Ctrl Pts',(66.114982666556,94.4109657890452,206.69999993673));
#25763=CARTESIAN_POINT('Ctrl Pts',(66.1225753392106,94.4169681229566,206.845179687536));
#25764=CARTESIAN_POINT('Ctrl Pts',(66.1311276201516,94.4237204506714,206.987155428366));
#25765=CARTESIAN_POINT('Ctrl Pts',(66.1458107299093,94.4352827739518,207.172140952524));
#25766=CARTESIAN_POINT('Ctrl Pts',(66.1507290952786,94.4391531397854,207.228982204513));
#25767=CARTESIAN_POINT('Ctrl Pts',(66.1567000620981,94.4438447214087,207.285548017371));
#25768=CARTESIAN_POINT('',(65.1689064613399,93.6082369448483,206.699999825671));
#25769=CARTESIAN_POINT('Origin',(77.215862801455,80.368869783441,206.7));
#25770=CARTESIAN_POINT('Ctrl Pts',(65.1296586956086,93.5724174245798,207.285548075353));
#25771=CARTESIAN_POINT('Ctrl Pts',(65.1353053901753,93.5775862704772,207.228541407465));
#25772=CARTESIAN_POINT('Ctrl Pts',(65.1399579139802,93.5818387450385,207.17122564234));
#25773=CARTESIAN_POINT('Ctrl Pts',(65.153736689073,93.5944243404895,206.986234752513));
#25774=CARTESIAN_POINT('Ctrl Pts',(65.1617661917048,93.6017397697266,206.84471856995));
#25775=CARTESIAN_POINT('Ctrl Pts',(65.1689047120699,93.6082353570854,206.699999668119));
#25776=CARTESIAN_POINT('Origin',(77.215862801455,80.368869783441,207.344186240766));
#25777=CARTESIAN_POINT('',(60.4296192316701,74.1534030434687,206.699999966494));
#25778=CARTESIAN_POINT('Ctrl Pts',(60.4296190734685,74.1534034691059,206.699999936224));
#25779=CARTESIAN_POINT('Ctrl Pts',(60.4262555077399,74.162487523505,206.845315153431));
#25780=CARTESIAN_POINT('Ctrl Pts',(60.4224746505866,74.1727180566403,206.987426060047));
#25781=CARTESIAN_POINT('Ctrl Pts',(60.4160156054915,74.1902646513169,207.172409754229));
#25782=CARTESIAN_POINT('Ctrl Pts',(60.4138599947734,74.1961265458095,207.229111613155));
#25783=CARTESIAN_POINT('Ctrl Pts',(60.4112505043822,74.2032387901793,207.285547584101));
#25784=CARTESIAN_POINT('',(60.9005109638373,73.0054945851509,206.699999827092));
#25785=CARTESIAN_POINT('Origin',(77.215862801455,80.368869783441,206.7));
#25786=CARTESIAN_POINT('',(60.9224377356629,72.9571021383096,207.285550046838));
#25787=CARTESIAN_POINT('Ctrl Pts',(60.9224424447625,72.957091786218,207.285548519515));
#25788=CARTESIAN_POINT('Ctrl Pts',(60.9192653221022,72.964076101594,207.228412061246));
#25789=CARTESIAN_POINT('Ctrl Pts',(60.9166543398919,72.969827192782,207.170956688005));
#25790=CARTESIAN_POINT('Ctrl Pts',(60.9089490604414,72.9868142803523,206.985964005474));
#25791=CARTESIAN_POINT('Ctrl Pts',(60.904478835706,72.9967027942644,206.844583002872));
#25792=CARTESIAN_POINT('Ctrl Pts',(60.9005119250647,73.0054924482591,206.699999670811));
#25793=CARTESIAN_POINT('',(60.95014735807,72.8964872239874,207.344186240766));
#25794=CARTESIAN_POINT('Ctrl Pts',(60.95014735807,72.8964872239874,207.344186240766));
#25795=CARTESIAN_POINT('Ctrl Pts',(60.9478299428105,72.9015317217597,207.344186240766));
#25796=CARTESIAN_POINT('Ctrl Pts',(60.9453166586466,72.9070093250897,207.343449242348));
#25797=CARTESIAN_POINT('Ctrl Pts',(60.9404808057933,72.9175628515142,207.340322634924));
#25798=CARTESIAN_POINT('Ctrl Pts',(60.9381582121413,72.9226387660393,207.337933035602));
#25799=CARTESIAN_POINT('Ctrl Pts',(60.9340879278448,72.9315428546402,207.332255389429));
#25800=CARTESIAN_POINT('Ctrl Pts',(60.932132684209,72.9358252668116,207.328654585832));
#25801=CARTESIAN_POINT('Ctrl Pts',(60.9286619592505,72.9434333401516,207.320274409274));
#25802=CARTESIAN_POINT('Ctrl Pts',(60.9271459728306,72.9467601852501,207.315496320451));
#25803=CARTESIAN_POINT('Ctrl Pts',(60.9241006297042,72.9534461421773,207.302683707375));
#25804=CARTESIAN_POINT('Ctrl Pts',(60.922915707046,72.9560514050313,207.294147623841));
#25805=CARTESIAN_POINT('Ctrl Pts',(60.9224377356548,72.9571021383274,207.285550046692));
#25806=CARTESIAN_POINT('',(77.8232478055421,62.47917768277,207.344186240766));
#25807=CARTESIAN_POINT('Origin',(77.215862801455,80.368869783441,207.344186240766));
#25808=CARTESIAN_POINT('',(77.889852177038,62.4815632844674,207.285548215602));
#25809=CARTESIAN_POINT('Ctrl Pts',(77.8898535835874,62.4815632107454,207.285548403908));
#25810=CARTESIAN_POINT('Ctrl Pts',(77.88870020223,62.4815197515247,207.294146535107));
#25811=CARTESIAN_POINT('Ctrl Pts',(77.885840089992,62.481411806529,207.302683220628));
#25812=CARTESIAN_POINT('Ctrl Pts',(77.8784980413168,62.4811387548963,207.315496320451));
#25813=CARTESIAN_POINT('Ctrl Pts',(77.8748445750857,62.4810034861528,207.320274409275));
#25814=CARTESIAN_POINT('Ctrl Pts',(77.8664878329066,62.4806975910132,207.328654585832));
#25815=CARTESIAN_POINT('Ctrl Pts',(77.861783272206,62.4805268857253,207.332255389429));
#25816=CARTESIAN_POINT('Ctrl Pts',(77.8519992485687,62.4801763296939,207.337933035602));
#25817=CARTESIAN_POINT('Ctrl Pts',(77.8464206987003,62.4799785143681,207.340322634924));
#25818=CARTESIAN_POINT('Ctrl Pts',(77.8348190503462,62.4795733621974,207.343449242348));
#25819=CARTESIAN_POINT('Ctrl Pts',(77.8287959483374,62.4793660515086,207.344186240766));
#25820=CARTESIAN_POINT('Ctrl Pts',(77.8232478055421,62.47917768277,207.344186240766));
#25821=CARTESIAN_POINT('',(77.9429269897965,62.483641866357,206.699999966761));
#25822=CARTESIAN_POINT('Ctrl Pts',(77.9429265397247,62.483641847502,206.699999936729));
#25823=CARTESIAN_POINT('Ctrl Pts',(77.9332558551646,62.4832487183737,206.845179687469));
#25824=CARTESIAN_POINT('Ctrl Pts',(77.9223679958966,62.4828128751116,206.987155428232));
#25825=CARTESIAN_POINT('Ctrl Pts',(77.9036929474648,62.4820892744566,207.172140952389));
#25826=CARTESIAN_POINT('Ctrl Pts',(77.89743896233,62.4818490253519,207.228982204448));
#25827=CARTESIAN_POINT('Ctrl Pts',(77.8898507061996,62.4815631023261,207.285548017369));
#25828=CARTESIAN_POINT('',(79.1801504439358,62.5769734833615,206.699999825671));
#25829=CARTESIAN_POINT('Origin',(77.215862801455,80.368869783441,206.7));
#25830=CARTESIAN_POINT('Ctrl Pts',(79.2329567391591,62.5828828261064,207.285548075332));
#25831=CARTESIAN_POINT('Ctrl Pts',(79.225350295901,62.5820201857243,207.228541407435));
#25832=CARTESIAN_POINT('Ctrl Pts',(79.219086783242,62.5813145464144,207.171225642298));
#25833=CARTESIAN_POINT('Ctrl Pts',(79.200541892634,62.5792315466046,206.986234752478));
#25834=CARTESIAN_POINT('Ctrl Pts',(79.1897459871301,62.5780328632611,206.844718569932));
#25835=CARTESIAN_POINT('Ctrl Pts',(79.1801527923866,62.5769737396933,206.69999966812));
#25836=CARTESIAN_POINT('',(94.419021870213,75.4230313252008,207.344186240766));
#25837=CARTESIAN_POINT('Origin',(77.215862801455,80.368869783441,207.344186240766));
#25838=CARTESIAN_POINT('',(94.4373172975837,75.4871179909361,207.285548914041));
#25839=CARTESIAN_POINT('Ctrl Pts',(94.4373177953928,75.4871192888155,207.285549099901));
#25840=CARTESIAN_POINT('Ctrl Pts',(94.4370030019744,75.4860087853819,207.294146996368));
#25841=CARTESIAN_POINT('Ctrl Pts',(94.4362226056726,75.4832551184153,207.302683426846));
#25842=CARTESIAN_POINT('Ctrl Pts',(94.4342154480476,75.4761875999915,207.315496320451));
#25843=CARTESIAN_POINT('Ctrl Pts',(94.4332160785974,75.4726708722743,207.320274409274));
#25844=CARTESIAN_POINT('Ctrl Pts',(94.4309268349098,75.4646279825559,207.328654585832));
#25845=CARTESIAN_POINT('Ctrl Pts',(94.4296366390347,75.4601005742151,207.332255389429));
#25846=CARTESIAN_POINT('Ctrl Pts',(94.4269491926396,75.4506863488119,207.337933035602));
#25847=CARTESIAN_POINT('Ctrl Pts',(94.4254149329567,75.4453192828758,207.340322634924));
#25848=CARTESIAN_POINT('Ctrl Pts',(94.4222182129065,75.4341593826194,207.343449242348));
#25849=CARTESIAN_POINT('Ctrl Pts',(94.4205557265731,75.428366553024,207.344186240766));
#25850=CARTESIAN_POINT('Ctrl Pts',(94.419021870213,75.4230313252008,207.344186240766));
#25851=CARTESIAN_POINT('',(94.4517290859501,75.5382473180358,206.699999967191));
#25852=CARTESIAN_POINT('Ctrl Pts',(94.4517289664912,75.5382468897594,206.699999937545));
#25853=CARTESIAN_POINT('Ctrl Pts',(94.4491205523975,75.528939958291,206.844960355996));
#25854=CARTESIAN_POINT('Ctrl Pts',(94.44617790075,75.5184654593862,206.986717295167));
#25855=CARTESIAN_POINT('Ctrl Pts',(94.44110395422,75.5004927769422,207.171705759969));
#25856=CARTESIAN_POINT('Ctrl Pts',(94.4393958410628,75.4944500502634,207.228772753636));
#25857=CARTESIAN_POINT('Ctrl Pts',(94.4373170203668,75.4871165547408,207.285548718384));
#25858=CARTESIAN_POINT('',(94.7449571171753,76.7438384229745,206.69999982336));
#25859=CARTESIAN_POINT('Origin',(77.215862801455,80.368869783441,206.7));
#25860=CARTESIAN_POINT('',(94.7556372114542,76.7958719320097,207.285548916829));
#25861=CARTESIAN_POINT('Ctrl Pts',(94.7556395308917,76.7958833180998,207.28554735655));
#25862=CARTESIAN_POINT('Ctrl Pts',(94.7541172320878,76.7884103591634,207.228750629597));
#25863=CARTESIAN_POINT('Ctrl Pts',(94.7528586977031,76.7822554461689,207.171660554524));
#25864=CARTESIAN_POINT('Ctrl Pts',(94.7491113652146,76.7639598982199,206.9866725855));
#25865=CARTESIAN_POINT('Ctrl Pts',(94.7469148396517,76.7533051195487,206.844937777645));
#25866=CARTESIAN_POINT('Ctrl Pts',(94.7449576048465,76.7438407664931,206.699999663745));
#25867=CARTESIAN_POINT('',(94.7688192182643,76.861203746089,207.344186240769));
#25868=CARTESIAN_POINT('Ctrl Pts',(94.7688192182643,76.861203746089,207.344186240766));
#25869=CARTESIAN_POINT('Ctrl Pts',(94.7677313833287,76.8557600353682,207.344186240766));
#25870=CARTESIAN_POINT('Ctrl Pts',(94.766547643411,76.8498507633878,207.343449242348));
#25871=CARTESIAN_POINT('Ctrl Pts',(94.7642617790702,76.8384693216063,207.340322634924));
#25872=CARTESIAN_POINT('Ctrl Pts',(94.7631596798826,76.8329971440765,207.337933035602));
#25873=CARTESIAN_POINT('Ctrl Pts',(94.7612231800783,76.8234002708056,207.332255389429));
#25874=CARTESIAN_POINT('Ctrl Pts',(94.7602899163563,76.8187860481728,207.328654585832));
#25875=CARTESIAN_POINT('Ctrl Pts',(94.7586295191669,76.8105902082001,207.320274409275));
#25876=CARTESIAN_POINT('Ctrl Pts',(94.7579020989926,76.8070073360248,207.315496320451));
#25877=CARTESIAN_POINT('Ctrl Pts',(94.7564390863843,76.7998074367317,207.302683372569));
#25878=CARTESIAN_POINT('Ctrl Pts',(94.7558676085502,76.7970029467077,207.294146874964));
#25879=CARTESIAN_POINT('Ctrl Pts',(94.7556372114512,76.7958719319941,207.285548916715));
#25880=CARTESIAN_POINT('Origin',(77.215862801455,80.368869783441,207.344186240766));
#25881=CARTESIAN_POINT('',(87.1362333696184,95.2684082920857,206.699999967189));
#25882=CARTESIAN_POINT('Ctrl Pts',(87.1362337400429,95.2684080461128,206.699999937541));
#25883=CARTESIAN_POINT('Ctrl Pts',(87.1442791135725,95.2630512969072,206.844960355813));
#25884=CARTESIAN_POINT('Ctrl Pts',(87.1533316246345,95.2570158707191,206.986717294808));
#25885=CARTESIAN_POINT('Ctrl Pts',(87.1688567256818,95.2466363964988,207.171705759608));
#25886=CARTESIAN_POINT('Ctrl Pts',(87.1740758642901,95.2431445791019,207.228772753463));
#25887=CARTESIAN_POINT('Ctrl Pts',(87.180408042097,95.2389013283705,207.28554871838));
#25888=CARTESIAN_POINT('',(86.0802605381687,95.9198328616278,206.699999823361));
#25889=CARTESIAN_POINT('Origin',(77.215862801455,80.368869783441,206.7));
#25890=CARTESIAN_POINT('',(86.0342766273764,95.946016145882,207.285410051862));
#25891=CARTESIAN_POINT('Ctrl Pts',(86.0340971970359,95.9460563761667,207.285262733977));
#25892=CARTESIAN_POINT('Ctrl Pts',(86.0407188285758,95.9423078752001,207.228559905421));
#25893=CARTESIAN_POINT('Ctrl Pts',(86.0461731162624,95.9392149023471,207.171573816788));
#25894=CARTESIAN_POINT('Ctrl Pts',(86.0624076112581,95.9300016641009,206.986672585795));
#25895=CARTESIAN_POINT('Ctrl Pts',(86.0718621442226,95.9246201364663,206.844937777794));
#25896=CARTESIAN_POINT('Ctrl Pts',(86.0802584600576,95.9198340496126,206.699999663746));
#25897=CARTESIAN_POINT('',(85.9760132775813,95.9787949477595,207.34418624088));
#25898=CARTESIAN_POINT('Ctrl Pts',(85.9760132775813,95.9787949477595,207.344186240766));
#25899=CARTESIAN_POINT('Ctrl Pts',(85.980854394653,95.9760781561302,207.344186240766));
#25900=CARTESIAN_POINT('Ctrl Pts',(85.9861086505249,95.9731262871016,207.343449242348));
#25901=CARTESIAN_POINT('Ctrl Pts',(85.9962266739679,95.9674352419939,207.340322634924));
#25902=CARTESIAN_POINT('Ctrl Pts',(86.0010904566875,95.9646960875269,207.337933035602));
#25903=CARTESIAN_POINT('Ctrl Pts',(86.0096192141986,95.9598887698357,207.332255389428));
#25904=CARTESIAN_POINT('Ctrl Pts',(86.0137192063509,95.9575753100821,207.328654585832));
#25905=CARTESIAN_POINT('Ctrl Pts',(86.0210008224145,95.9534635246808,207.320274409274));
#25906=CARTESIAN_POINT('Ctrl Pts',(86.024183551148,95.9516645385931,207.315496320451));
#25907=CARTESIAN_POINT('Ctrl Pts',(86.0306209260497,95.9480245135938,207.302599308419));
#25908=CARTESIAN_POINT('Ctrl Pts',(86.0331233851216,95.9466076511945,207.293958732845));
#25909=CARTESIAN_POINT('Ctrl Pts',(86.0341066806811,95.946051007478,207.285265181889));
#25910=CARTESIAN_POINT('Origin',(77.215862801455,80.368869783441,207.344186240766));
#25911=CARTESIAN_POINT('Origin',(77.215862801455,80.368869783441,197.7));
#25912=CARTESIAN_POINT('',(77.807098035462,62.6991535162084,201.741111932487));
#25913=CARTESIAN_POINT('',(61.1539813020695,72.980744529632,201.741111932425));
#25914=CARTESIAN_POINT('Origin',(77.215862801455,80.368869783441,201.741111932358));
#25915=CARTESIAN_POINT('Ctrl Pts',(60.9005100041822,73.0054967262931,206.699999797758));
#25916=CARTESIAN_POINT('Ctrl Pts',(60.9383106449015,73.0111068965595,205.87285383463));
#25917=CARTESIAN_POINT('Ctrl Pts',(60.9765983511668,73.0156536991714,205.045723649382));
#25918=CARTESIAN_POINT('Ctrl Pts',(61.036177641715,73.017794419973,203.805110977245));
#25919=CARTESIAN_POINT('Ctrl Pts',(61.056362889984,73.0177980538245,203.391593008183));
#25920=CARTESIAN_POINT('Ctrl Pts',(61.0881220477898,73.0145739609718,202.771407903025));
#25921=CARTESIAN_POINT('Ctrl Pts',(61.0989324419101,73.0130108881507,202.564693369105));
#25922=CARTESIAN_POINT('Ctrl Pts',(61.1161852013738,73.0084051153063,202.254685622264));
#25923=CARTESIAN_POINT('Ctrl Pts',(61.1220930802366,73.0065284737844,202.151351857905));
#25924=CARTESIAN_POINT('Ctrl Pts',(61.1316846267869,73.0021175223093,201.996443305138));
#25925=CARTESIAN_POINT('Ctrl Pts',(61.1349921347903,73.0004066620236,201.944814005535));
#25926=CARTESIAN_POINT('Ctrl Pts',(61.1404702932454,72.9967068289114,201.86746331438));
#25927=CARTESIAN_POINT('Ctrl Pts',(61.1423745128547,72.9953029618212,201.841686059695));
#25928=CARTESIAN_POINT('Ctrl Pts',(61.1455990957178,72.9923866534762,201.803113993957));
#25929=CARTESIAN_POINT('Ctrl Pts',(61.1467287621209,72.9912937104118,201.790272644151));
#25930=CARTESIAN_POINT('Ctrl Pts',(61.1486890600559,72.9890682219378,201.771088244947));
#25931=CARTESIAN_POINT('Ctrl Pts',(61.1493825770163,72.9882385880473,201.764699691419));
#25932=CARTESIAN_POINT('Ctrl Pts',(61.1506142386167,72.9865676498396,201.755215001631));
#25933=CARTESIAN_POINT('Ctrl Pts',(61.1510536238296,72.9859469806554,201.752062963043));
#25934=CARTESIAN_POINT('Ctrl Pts',(61.1521195445798,72.9842847677176,201.745890878911));
#25935=CARTESIAN_POINT('Ctrl Pts',(61.1526220601575,72.9836995364303,201.741111962039));
#25936=CARTESIAN_POINT('Ctrl Pts',(61.1539813021289,72.9807445296591,201.741111932358));
#25937=CARTESIAN_POINT('',(60.5926319978065,74.3491829381161,201.741111932489));
#25938=CARTESIAN_POINT('Ctrl Pts',(60.5926319978361,74.3491829381273,201.741111932358));
#25939=CARTESIAN_POINT('Ctrl Pts',(60.5937393175791,74.3461250955133,201.741111963319));
#25940=CARTESIAN_POINT('Ctrl Pts',(60.5937927553975,74.3453549761292,201.745890861414));
#25941=CARTESIAN_POINT('Ctrl Pts',(60.5942012600518,74.3434228683981,201.752062897732));
#25942=CARTESIAN_POINT('Ctrl Pts',(60.594324352301,74.3426723409001,201.75521490968));
#25943=CARTESIAN_POINT('Ctrl Pts',(60.5946210288793,74.3406175201717,201.764699543009));
#25944=CARTESIAN_POINT('Ctrl Pts',(60.5947099819196,74.3395396558076,201.771088063263));
#25945=CARTESIAN_POINT('Ctrl Pts',(60.5948774701612,74.3365780380361,201.790272386922));
#25946=CARTESIAN_POINT('Ctrl Pts',(60.5948409011576,74.3350062230635,201.80311369854));
#25947=CARTESIAN_POINT('Ctrl Pts',(60.5945936658665,74.3306643267586,201.841685661127));
#25948=CARTESIAN_POINT('Ctrl Pts',(60.5942241686695,74.3283268124689,201.867462868231));
#25949=CARTESIAN_POINT('Ctrl Pts',(60.5929232339402,74.3218432894536,201.944813434034));
#25950=CARTESIAN_POINT('Ctrl Pts',(60.5917705844262,74.3183009330135,201.996442677713));
#25951=CARTESIAN_POINT('Ctrl Pts',(60.5880415026138,74.3084200407889,202.151351090415));
#25952=CARTESIAN_POINT('Ctrl Pts',(60.5851546003288,74.3029318988099,202.254684800762));
#25953=CARTESIAN_POINT('Ctrl Pts',(60.5761099141485,74.2875272696542,202.56469242477));
#25954=CARTESIAN_POINT('Ctrl Pts',(60.5695137820587,74.2788162752227,202.771406933039));
#25955=CARTESIAN_POINT('Ctrl Pts',(60.5491749431726,74.2541982851575,203.391592016162));
#25956=CARTESIAN_POINT('Ctrl Pts',(60.5348068091768,74.2400125818057,203.805110051126));
#25957=CARTESIAN_POINT('Ctrl Pts',(60.490901938456,74.1996574574576,205.045723068922));
#25958=CARTESIAN_POINT('Ctrl Pts',(60.4604606428822,74.1759805013104,205.872853625126));
#25959=CARTESIAN_POINT('Ctrl Pts',(60.4296193906672,74.1534026174594,206.699999960794));
#25960=CARTESIAN_POINT('',(65.2237133691081,93.3595119561188,201.741111932425));
#25961=CARTESIAN_POINT('Origin',(77.215862801455,80.368869783441,201.741111932358));
#25962=CARTESIAN_POINT('Ctrl Pts',(65.1689082151754,93.6082385324285,206.69999979608));
#25963=CARTESIAN_POINT('Ctrl Pts',(65.1859267393918,93.5740209471359,205.872853767758));
#25964=CARTESIAN_POINT('Ctrl Pts',(65.202084596116,93.5390113872842,205.045723525105));
#25965=CARTESIAN_POINT('Ctrl Pts',(65.2225352272511,93.483007739342,203.805110800395));
#25966=CARTESIAN_POINT('Ctrl Pts',(65.2287775850782,93.4638108194459,203.391592818749));
#25967=CARTESIAN_POINT('Ctrl Pts',(65.2355278034753,93.4326082192978,202.771407717802));
#25968=CARTESIAN_POINT('Ctrl Pts',(65.2373826894445,93.4218433237596,202.564693188781));
#25969=CARTESIAN_POINT('Ctrl Pts',(65.2383353173637,93.4040105223618,202.2546854654));
#25970=CARTESIAN_POINT('Ctrl Pts',(65.2383767315617,93.3978114373734,202.151351711356));
#25971=CARTESIAN_POINT('Ctrl Pts',(65.2371466798792,93.3873253878303,201.996443185339));
#25972=CARTESIAN_POINT('Ctrl Pts',(65.2365420159416,93.3836507465764,201.944813896416));
#25973=CARTESIAN_POINT('Ctrl Pts',(65.2347168317198,93.3772967459819,201.8674632292));
#25974=CARTESIAN_POINT('Ctrl Pts',(65.233970373536,93.3750516660578,201.841685983602));
#25975=CARTESIAN_POINT('Ctrl Pts',(65.2321937479147,93.3710832436713,201.803113937563));
#25976=CARTESIAN_POINT('Ctrl Pts',(65.2315035646884,93.369670954703,201.79027259505));
#25977=CARTESIAN_POINT('Ctrl Pts',(65.2299931117319,93.3671185443332,201.771088210274));
#25978=CARTESIAN_POINT('Ctrl Pts',(65.2294185185355,93.3662024733727,201.764699663099));
#25979=CARTESIAN_POINT('Ctrl Pts',(65.2282102113793,93.3645144973317,201.755214984094));
#25980=CARTESIAN_POINT('Ctrl Pts',(65.2277557874688,93.3639047286458,201.752062950593));
#25981=CARTESIAN_POINT('Ctrl Pts',(65.2265045506743,93.3623770854172,201.745890875594));
#25982=CARTESIAN_POINT('Ctrl Pts',(65.2261032722959,93.3617181671861,201.741111962317));
#25983=CARTESIAN_POINT('Ctrl Pts',(65.2237133691526,93.3595119560702,201.741111932358));
#25984=CARTESIAN_POINT('',(66.3515448153964,94.3164511782291,201.741111932487));
#25985=CARTESIAN_POINT('Ctrl Pts',(66.3515448154396,94.3164511781742,201.741111932358));
#25986=CARTESIAN_POINT('Ctrl Pts',(66.3489790895714,94.3144526354332,201.741111963088));
#25987=CARTESIAN_POINT('Ctrl Pts',(66.3482633166899,94.314163781558,201.745890864771));
#25988=CARTESIAN_POINT('Ctrl Pts',(66.3465522068942,94.3131779463266,201.752062910219));
#25989=CARTESIAN_POINT('Ctrl Pts',(66.3458765257224,94.3128288491502,201.755214927256));
#25990=CARTESIAN_POINT('Ctrl Pts',(66.3440141578885,94.3119114361031,201.764699571368));
#25991=CARTESIAN_POINT('Ctrl Pts',(66.3430166397612,94.3114936124396,201.771088097978));
#25992=CARTESIAN_POINT('Ctrl Pts',(66.3402520120046,94.310418733184,201.790272436065));
#25993=CARTESIAN_POINT('Ctrl Pts',(66.3387459692438,94.3099675874997,201.803113754976));
#25994=CARTESIAN_POINT('Ctrl Pts',(66.3345405662682,94.308860434356,201.841685737264));
#25995=CARTESIAN_POINT('Ctrl Pts',(66.332203471895,94.3084892170732,201.867462953456));
#25996=CARTESIAN_POINT('Ctrl Pts',(66.3256357889722,94.3077221418656,201.9448135432));
#25997=CARTESIAN_POINT('Ctrl Pts',(66.3219108818743,94.3077232949242,201.99644279756));
#25998=CARTESIAN_POINT('Ctrl Pts',(66.3113619485989,94.3082153062037,202.151351237013));
#25999=CARTESIAN_POINT('Ctrl Pts',(66.3052506589714,94.3092643477764,202.254684957675));
#26000=CARTESIAN_POINT('Ctrl Pts',(66.2878059414537,94.3131043070356,202.564692605142));
#26001=CARTESIAN_POINT('Ctrl Pts',(66.2774834127232,94.3166848106869,202.77140711831));
#26002=CARTESIAN_POINT('Ctrl Pts',(66.247786403833,94.3284182028902,203.39159220564));
#26003=CARTESIAN_POINT('Ctrl Pts',(66.2298555084119,94.3376980668689,203.805110228017));
#26004=CARTESIAN_POINT('Ctrl Pts',(66.1779094279662,94.3669797255545,205.045723192665));
#26005=CARTESIAN_POINT('Ctrl Pts',(66.1459849127475,94.3886123873169,205.872853690893));
#26006=CARTESIAN_POINT('Ctrl Pts',(66.1149819603839,94.4109652285824,206.699999961109));
#26007=CARTESIAN_POINT('',(81.3941453425875,97.5476470120627,201.741111932492));
#26008=CARTESIAN_POINT('Origin',(77.215862801455,80.368869783441,201.741111932358));
#26009=CARTESIAN_POINT('',(83.0552394877203,97.0562935504538,201.741111932358));
#26010=CARTESIAN_POINT('Origin',(77.215862801455,80.368869783441,201.741111932358));
#26011=CARTESIAN_POINT('',(82.9959179641957,96.8867680249146,197.7));
#26012=CARTESIAN_POINT('',(85.8606360184079,95.7908128547202,201.741111932426));
#26013=CARTESIAN_POINT('Origin',(77.215862801455,80.368869783441,201.741111932358));
#26014=CARTESIAN_POINT('Ctrl Pts',(86.0802626175339,95.9198316691863,206.699999793354));
#26015=CARTESIAN_POINT('Ctrl Pts',(86.0529786776688,95.893069019184,205.872853659539));
#26016=CARTESIAN_POINT('Ctrl Pts',(86.0246754069566,95.8668798833011,205.045723323998));
#26017=CARTESIAN_POINT('Ctrl Pts',(85.9777312853402,95.8301174987039,203.805110514213));
#26018=CARTESIAN_POINT('Ctrl Pts',(85.961402457991,95.8182460959664,203.391592512203));
#26019=CARTESIAN_POINT('Ctrl Pts',(85.9338117707789,95.8021796651052,202.771407418065));
#26020=CARTESIAN_POINT('Ctrl Pts',(85.9241464704097,95.7970874106423,202.56469289697));
#26021=CARTESIAN_POINT('Ctrl Pts',(85.9074798068452,95.7906677381534,202.254685211545));
#26022=CARTESIAN_POINT('Ctrl Pts',(85.901596526642,95.788711626652,202.151351474192));
#26023=CARTESIAN_POINT('Ctrl Pts',(85.8912427589881,95.7866390298392,201.996442991456));
#26024=CARTESIAN_POINT('Ctrl Pts',(85.8875608017384,95.7860778159899,201.944813719815));
#26025=CARTESIAN_POINT('Ctrl Pts',(85.880953134623,95.785848738158,201.867463091334));
#26026=CARTESIAN_POINT('Ctrl Pts',(85.8785870294705,95.7858643697771,201.841685860439));
#26027=CARTESIAN_POINT('Ctrl Pts',(85.8742633490481,95.7863267288807,201.803113846275));
#26028=CARTESIAN_POINT('Ctrl Pts',(85.8727067264141,95.7865463446168,201.790272515562));
#26029=CARTESIAN_POINT('Ctrl Pts',(85.8698121308553,95.787193427246,201.771088154131));
#26030=CARTESIAN_POINT('Ctrl Pts',(85.8687632059339,95.7874565578042,201.764699617238));
#26031=CARTESIAN_POINT('Ctrl Pts',(85.8667841989931,95.7880836116175,201.75521495568));
#26032=CARTESIAN_POINT('Ctrl Pts',(85.8660637545444,95.7883271813326,201.75206293041));
#26033=CARTESIAN_POINT('Ctrl Pts',(85.8642239733752,95.7890446301688,201.745890870187));
#26034=CARTESIAN_POINT('Ctrl Pts',(85.8634730846983,95.7892225381229,201.741111962688));
#26035=CARTESIAN_POINT('Ctrl Pts',(85.8606360183751,95.7908128546621,201.741111932358));
#26036=CARTESIAN_POINT('',(87.1194741084993,95.014241582934,201.741111932485));
#26037=CARTESIAN_POINT('Ctrl Pts',(87.119474108461,95.0142415828767,201.741111932358));
#26038=CARTESIAN_POINT('Ctrl Pts',(87.1167799038052,95.0160634812828,201.741111962705));
#26039=CARTESIAN_POINT('Ctrl Pts',(87.1162839950345,95.0166547167802,201.745890870188));
#26040=CARTESIAN_POINT('Ctrl Pts',(87.1148173319683,95.0179769977751,201.752062930411));
#26041=CARTESIAN_POINT('Ctrl Pts',(87.1142764019131,95.0185115640335,201.755214955681));
#26042=CARTESIAN_POINT('Ctrl Pts',(87.112828054955,95.0199988286518,201.76469961724));
#26043=CARTESIAN_POINT('Ctrl Pts',(87.1121222584439,95.0208181774568,201.771088154132));
#26044=CARTESIAN_POINT('Ctrl Pts',(87.1102451985936,95.0231147065111,201.790272515564));
#26045=CARTESIAN_POINT('Ctrl Pts',(87.1093504930545,95.0244073035463,201.803113846276));
#26046=CARTESIAN_POINT('Ctrl Pts',(87.1069973056896,95.0280638726432,201.84168586044));
#26047=CARTESIAN_POINT('Ctrl Pts',(87.1059216935689,95.0301714201536,201.867463091335));
#26048=CARTESIAN_POINT('Ctrl Pts',(87.1031616387417,95.0361794014043,201.944813719816));
#26049=CARTESIAN_POINT('Ctrl Pts',(87.1020111401724,95.0397217344228,201.996442991457));
#26050=CARTESIAN_POINT('Ctrl Pts',(87.0992177879608,95.0499047273817,202.151351474193));
#26051=CARTESIAN_POINT('Ctrl Pts',(87.0983261869635,95.0560402310952,202.254685211547));
#26052=CARTESIAN_POINT('Ctrl Pts',(87.0965852479142,95.0738154666901,202.564692896971));
#26053=CARTESIAN_POINT('Ctrl Pts',(87.0967994361659,95.0847380675769,202.771407418066));
#26054=CARTESIAN_POINT('Ctrl Pts',(87.0987782199621,95.1166043606802,203.391592512204));
#26055=CARTESIAN_POINT('Ctrl Pts',(87.1020610131019,95.1365238003,203.805110514214));
#26056=CARTESIAN_POINT('Ctrl Pts',(87.1138518873724,95.1949720607912,205.045723392875));
#26057=CARTESIAN_POINT('Ctrl Pts',(87.1245574910124,95.2320171179916,205.872853797301));
#26058=CARTESIAN_POINT('Ctrl Pts',(87.1362329983495,95.2684085378955,206.699999961615));
#26059=CARTESIAN_POINT('',(94.5543840898835,76.9128443788708,201.741111932426));
#26060=CARTESIAN_POINT('Origin',(77.215862801455,80.368869783441,201.741111932358));
#26061=CARTESIAN_POINT('Ctrl Pts',(94.7449566256531,76.7438360768859,206.699999793353));
#26062=CARTESIAN_POINT('Ctrl Pts',(94.7110726318838,76.7615145320216,205.87285365954));
#26063=CARTESIAN_POINT('Ctrl Pts',(94.6774190919,76.7803396540104,205.045723324001));
#26064=CARTESIAN_POINT('Ctrl Pts',(94.6279494551094,76.8136259651829,203.805110514219));
#26065=CARTESIAN_POINT('Ctrl Pts',(94.6116131950293,76.8254871376443,203.39159251221));
#26066=CARTESIAN_POINT('Ctrl Pts',(94.5878071200303,76.846762640332,202.771407418073));
#26067=CARTESIAN_POINT('Ctrl Pts',(94.579977356171,76.8543812940616,202.564692896978));
#26068=CARTESIAN_POINT('Ctrl Pts',(94.5687216025371,76.8682484451523,202.254685211554));
#26069=CARTESIAN_POINT('Ctrl Pts',(94.5650431963817,76.8732393054302,202.151351474201));
#26070=CARTESIAN_POINT('Ctrl Pts',(94.5598725495164,76.8824458559882,201.996442991466));
#26071=CARTESIAN_POINT('Ctrl Pts',(94.5582010160652,76.8857741808062,201.944813719824));
#26072=CARTESIAN_POINT('Ctrl Pts',(94.5559412686686,76.8919876567305,201.867463091344));
#26073=CARTESIAN_POINT('Ctrl Pts',(94.5552249685192,76.8942427868902,201.841685860449));
#26074=CARTESIAN_POINT('Ctrl Pts',(94.5543286074288,76.8984977281506,201.803113846285));
#26075=CARTESIAN_POINT('Ctrl Pts',(94.554056451558,76.9000460292448,201.790272515572));
#26076=CARTESIAN_POINT('Ctrl Pts',(94.5537773844895,76.902998912742,201.771088154141));
#26077=CARTESIAN_POINT('Ctrl Pts',(94.553703500895,76.9040778114373,201.764699617248));
#26078=CARTESIAN_POINT('Ctrl Pts',(94.5536883177333,76.9061537291684,201.75521495569));
#26079=CARTESIAN_POINT('Ctrl Pts',(94.5536973367198,76.9069141797371,201.75206293042));
#26080=CARTESIAN_POINT('Ctrl Pts',(94.5538111474632,76.9088856194884,201.745890870196));
#26081=CARTESIAN_POINT('Ctrl Pts',(94.5537483106129,76.9096547335994,201.741111962713));
#26082=CARTESIAN_POINT('Ctrl Pts',(94.5543840898181,76.912844378884,201.741111932358));
#26083=CARTESIAN_POINT('',(94.2048232844883,75.4756444900036,201.741111932485));
#26084=CARTESIAN_POINT('Ctrl Pts',(94.2048232844219,75.4756444900223,201.741111932358));
#26085=CARTESIAN_POINT('Ctrl Pts',(94.20572345773,75.4787698284284,201.741111962672));
#26086=CARTESIAN_POINT('Ctrl Pts',(94.2061325118859,75.4794241675821,201.745890870179));
#26087=CARTESIAN_POINT('Ctrl Pts',(94.2069368520303,75.4812276543486,201.752062930403));
#26088=CARTESIAN_POINT('Ctrl Pts',(94.207278098174,75.4819072994615,201.755214955672));
#26089=CARTESIAN_POINT('Ctrl Pts',(94.208245007057,75.4837443493165,201.764699617231));
#26090=CARTESIAN_POINT('Ctrl Pts',(94.2088061509609,75.4846687943932,201.771088154123));
#26091=CARTESIAN_POINT('Ctrl Pts',(94.2104102364897,75.4871636509014,201.790272515555));
#26092=CARTESIAN_POINT('Ctrl Pts',(94.2113630901064,75.4884140008851,201.803113846268));
#26093=CARTESIAN_POINT('Ctrl Pts',(94.2141135190867,75.4917819570548,201.841685860432));
#26094=CARTESIAN_POINT('Ctrl Pts',(94.2157855334549,75.4934561929679,201.867463091327));
#26095=CARTESIAN_POINT('Ctrl Pts',(94.2206465593263,75.4979377294053,201.944813719807));
#26096=CARTESIAN_POINT('Ctrl Pts',(94.2236599946165,75.5001265596694,201.996442991449));
#26097=CARTESIAN_POINT('Ctrl Pts',(94.2324814031209,75.505929913371,202.151351474185));
#26098=CARTESIAN_POINT('Ctrl Pts',(94.2380410940483,75.5086738512261,202.254685211539));
#26099=CARTESIAN_POINT('Ctrl Pts',(94.2544083679373,75.5158224325321,202.564692896964));
#26100=CARTESIAN_POINT('Ctrl Pts',(94.2648625664955,75.5189939966968,202.771407418059));
#26101=CARTESIAN_POINT('Ctrl Pts',(94.2957806900231,75.5269592875904,203.391592512198));
#26102=CARTESIAN_POINT('Ctrl Pts',(94.3157396417436,75.5299926111441,203.805110514209));
#26103=CARTESIAN_POINT('Ctrl Pts',(94.3749708212775,75.536840329118,205.045723392872));
#26104=CARTESIAN_POINT('Ctrl Pts',(94.4135109777832,75.5381062472439,205.872853797299));
#26105=CARTESIAN_POINT('Ctrl Pts',(94.4517292049929,75.5382477470648,206.699999961618));
#26106=CARTESIAN_POINT('',(79.2820076043964,62.8104109182795,201.741111932425));
#26107=CARTESIAN_POINT('Origin',(77.215862801455,80.368869783441,201.741111932358));
#26108=CARTESIAN_POINT('Ctrl Pts',(79.1801480918987,62.5769732298611,206.699999796081));
#26109=CARTESIAN_POINT('Ctrl Pts',(79.1864924085904,62.614659075419,205.872853767758));
#26110=CARTESIAN_POINT('Ctrl Pts',(79.1939985308776,62.6524797541957,205.045723525105));
#26111=CARTESIAN_POINT('Ctrl Pts',(79.2103717410791,62.7098082365092,203.805110800395));
#26112=CARTESIAN_POINT('Ctrl Pts',(79.2166052339168,62.7290080368152,203.391592818749));
#26113=CARTESIAN_POINT('Ctrl Pts',(79.2294846207187,62.7582191494274,202.771407717802));
#26114=CARTESIAN_POINT('Ctrl Pts',(79.2343114332871,62.7680184074779,202.564693188781));
#26115=CARTESIAN_POINT('Ctrl Pts',(79.2440225987803,62.783005387508,202.254685465399));
#26116=CARTESIAN_POINT('Ctrl Pts',(79.2476328247242,62.7880448952679,202.151351711356));
#26117=CARTESIAN_POINT('Ctrl Pts',(79.2547915027158,62.7958052813137,201.996443185338));
#26118=CARTESIAN_POINT('Ctrl Pts',(79.2574405860539,62.7984227159912,201.944813896416));
#26119=CARTESIAN_POINT('Ctrl Pts',(79.2626519789498,62.8024903940862,201.8674632292));
#26120=CARTESIAN_POINT('Ctrl Pts',(79.2645755011755,62.8038679447865,201.841685983602));
#26121=CARTESIAN_POINT('Ctrl Pts',(79.2683454016495,62.806034191599,201.803113937563));
#26122=CARTESIAN_POINT('Ctrl Pts',(79.2697338942366,62.8067710778536,201.790272595049));
#26123=CARTESIAN_POINT('Ctrl Pts',(79.2724561455209,62.8079481992474,201.771088210274));
#26124=CARTESIAN_POINT('Ctrl Pts',(79.2734594541819,62.8083515788154,201.764699663099));
#26125=CARTESIAN_POINT('Ctrl Pts',(79.2754291626288,62.809006954992,201.755214984094));
#26126=CARTESIAN_POINT('Ctrl Pts',(79.2761552123347,62.8092331645485,201.752062950592));
#26127=CARTESIAN_POINT('Ctrl Pts',(79.2780654103254,62.8097335953468,201.745890875593));
#26128=CARTESIAN_POINT('Ctrl Pts',(79.2787773537758,62.8100308058813,201.741111962317));
#26129=CARTESIAN_POINT('Ctrl Pts',(79.282007604389,62.8104109183449,201.741111932358));
#26130=CARTESIAN_POINT('Ctrl Pts',(77.8070980354593,62.6991535162783,201.741111932358));
#26131=CARTESIAN_POINT('Ctrl Pts',(77.8103484652123,62.6992622754927,201.741111963075));
#26132=CARTESIAN_POINT('Ctrl Pts',(77.8110973217177,62.6990752424435,201.745890864766));
#26133=CARTESIAN_POINT('Ctrl Pts',(77.8130610980324,62.6988670347964,201.752062910214));
#26134=CARTESIAN_POINT('Ctrl Pts',(77.8138129297545,62.6987523049169,201.755214927251));
#26135=CARTESIAN_POINT('Ctrl Pts',(77.8158588588416,62.6983998353157,201.764699571363));
#26136=CARTESIAN_POINT('Ctrl Pts',(77.8169114585462,62.698151535316,201.771088097973));
#26137=CARTESIAN_POINT('Ctrl Pts',(77.8197798875591,62.6973961234773,201.790272436059));
#26138=CARTESIAN_POINT('Ctrl Pts',(77.821263478527,62.6968758782787,201.803113754971));
#26139=CARTESIAN_POINT('Ctrl Pts',(77.8253164892923,62.6952997101382,201.841685737259));
#26140=CARTESIAN_POINT('Ctrl Pts',(77.8274254344019,62.6942263216229,201.867462953451));
#26141=CARTESIAN_POINT('Ctrl Pts',(77.8331896769943,62.690986511338,201.944813543195));
#26142=CARTESIAN_POINT('Ctrl Pts',(77.8362025123878,62.6887961330358,201.996442797555));
#26143=CARTESIAN_POINT('Ctrl Pts',(77.8444475817057,62.6821975801426,202.151351237008));
#26144=CARTESIAN_POINT('Ctrl Pts',(77.8487751077061,62.6777567617667,202.25468495767));
#26145=CARTESIAN_POINT('Ctrl Pts',(77.860631109217,62.664396421781,202.564692605138));
#26146=CARTESIAN_POINT('Ctrl Pts',(77.8668776431422,62.6554323033246,202.771407118306));
#26147=CARTESIAN_POINT('Ctrl Pts',(77.884006313118,62.6284843257675,203.391592205636));
#26148=CARTESIAN_POINT('Ctrl Pts',(77.8930581450468,62.6104372422142,203.805110228014));
#26149=CARTESIAN_POINT('Ctrl Pts',(77.9178720797775,62.5562147427134,205.045723192663));
#26150=CARTESIAN_POINT('Ctrl Pts',(77.9309841955656,62.5199487924835,205.872853690892));
#26151=CARTESIAN_POINT('Ctrl Pts',(77.9429274404634,62.4836418858484,206.699999961109));
#26152=CARTESIAN_POINT('Origin',(93.7337610429286,74.5888146207003,197.7));
#26153=CARTESIAN_POINT('Origin',(77.215862801455,80.368869783441,209.7));
#26154=CARTESIAN_POINT('',(82.4344268912437,95.2821721957428,209.7));
#26155=CARTESIAN_POINT('Origin',(92.1291652137568,75.1503056936523,207.5));
#26156=CARTESIAN_POINT('Origin',(77.215862801455,80.368869783441,209.7));
#26157=CARTESIAN_POINT('',(80.5848092391667,89.9964447584713,209.7));
#26158=CARTESIAN_POINT('Origin',(86.8434377764853,76.9999233457293,210.));
#26159=CARTESIAN_POINT('',(81.344473631984,92.1673685273507,210.));
#26160=CARTESIAN_POINT('Origin',(77.215862801455,80.368869783441,210.));
#26161=CARTESIAN_POINT('Origin',(77.215862801455,80.368869783441,209.7));
#26162=CARTESIAN_POINT('',(81.344473631984,92.1673685273507,209.7));
#26163=CARTESIAN_POINT('Origin',(77.215862801455,80.368869783441,209.4));
#26164=CARTESIAN_POINT('',(66.8117635085218,50.6366529487886,209.4));
#26165=CARTESIAN_POINT('Origin',(106.948079636107,69.9647704905078,208.1));
#26166=CARTESIAN_POINT('Origin',(77.215862801455,80.368869783441,194.026481344607));
#26167=CARTESIAN_POINT('',(69.7713582305978,49.7612015989078,194.026481344607));
#26168=CARTESIAN_POINT('',(84.6603673723122,110.976537967974,194.026481344607));
#26169=CARTESIAN_POINT('Origin',(77.215862801455,80.368869783441,194.026481344607));
#26170=CARTESIAN_POINT('Origin',(77.215862801455,80.368869783441,194.026481344607));
#26171=CARTESIAN_POINT('',(84.6012840027022,110.73361996651,193.776481344607));
#26172=CARTESIAN_POINT('Origin',(84.6012840027022,110.73361996651,194.026481344607));
#26173=CARTESIAN_POINT('Origin',(77.215862801455,80.368869783441,193.776481344607));
#26174=CARTESIAN_POINT('Origin',(77.215862801455,80.368869783441,195.376481344607));
#26175=CARTESIAN_POINT('',(72.5482766022668,61.1783476677416,195.126481344607));
#26176=CARTESIAN_POINT('Origin',(77.215862801455,80.368869783441,195.126481344607));
#26177=CARTESIAN_POINT('',(72.6073599718767,61.4212656692062,195.376481344607));
#26178=CARTESIAN_POINT('Origin',(72.5482766022668,61.1783476677416,195.376481344607));
#26179=CARTESIAN_POINT('Origin',(77.215862801455,80.368869783441,195.376481344607));
#26180=CARTESIAN_POINT('Origin',(77.215862801455,80.368869783441,197.021721166268));
#26181=CARTESIAN_POINT('',(73.0800269287566,63.3646096809226,197.021721166268));
#26182=CARTESIAN_POINT('',(81.3516986741534,97.3731298859594,197.021721166268));
#26183=CARTESIAN_POINT('Origin',(77.215862801455,80.368869783441,197.021721166268));
#26184=CARTESIAN_POINT('Origin',(77.215862801455,80.368869783441,197.021721166268));
#26185=CARTESIAN_POINT('',(81.3517414998324,97.3733059613665,197.031238072604));
#26186=CARTESIAN_POINT('Origin',(81.4107820437634,97.616047887424,197.021721166268));
#26187=CARTESIAN_POINT('Origin',(77.215862801455,80.368869783441,197.031238072604));
#26188=CARTESIAN_POINT('Origin',(87.0652037611821,97.7633458837792,207.276481344607));
#26189=CARTESIAN_POINT('',(86.0937896005589,96.188663441779,207.526481344607));
#26190=CARTESIAN_POINT('',(79.7412900434344,85.8911302979345,207.526481344607));
#26191=CARTESIAN_POINT('',(86.3065605834827,96.0574060274146,207.276481344607));
#26192=CARTESIAN_POINT('Origin',(86.0937896005589,96.188663441779,207.276481344607));
#26193=CARTESIAN_POINT('',(87.277974744106,97.6320884694148,207.276481344607));
#26194=CARTESIAN_POINT('Origin',(86.0937896005589,96.188663441779,207.276481344607));
#26195=CARTESIAN_POINT('Origin',(86.0937896005589,96.188663441779,207.276481344607));
#26196=CARTESIAN_POINT('Origin',(86.0937896005589,96.188663441779,207.276481344607));
#26197=CARTESIAN_POINT('Origin',(77.215862801455,80.368869783441,207.276481344607));
#26198=CARTESIAN_POINT('',(66.0612008874025,94.6747068168279,207.526481344607));
#26199=CARTESIAN_POINT('Origin',(77.215862801455,80.368869783441,207.526481344607));
#26200=CARTESIAN_POINT('Origin',(66.0612008874025,94.6747068168279,207.276481344607));
#26201=CARTESIAN_POINT('Origin',(85.9930972697295,96.0254382715203,202.246481277241));
#26202=CARTESIAN_POINT('',(85.7715372937515,95.6461913480132,197.285998193683));
#26203=CARTESIAN_POINT('',(85.7715371009377,95.6461914584938,197.285998250943));
#26204=CARTESIAN_POINT('',(86.1109957253458,95.7403933688821,197.526481344568));
#26205=CARTESIAN_POINT('Ctrl Pts',(85.7715374871662,95.646191237174,197.285998135919));
#26206=CARTESIAN_POINT('Ctrl Pts',(85.7725054328388,95.6456968118517,197.28708943318));
#26207=CARTESIAN_POINT('Ctrl Pts',(85.7727762193796,95.6455685834453,197.287529424681));
#26208=CARTESIAN_POINT('Ctrl Pts',(85.775448730368,95.6442257365666,197.290389369077));
#26209=CARTESIAN_POINT('Ctrl Pts',(85.7811525394671,95.6413790023973,197.296803694516));
#26210=CARTESIAN_POINT('Ctrl Pts',(85.8294132680089,95.6211973451069,197.348830628001));
#26211=CARTESIAN_POINT('Ctrl Pts',(85.8738913768775,95.6148707634768,197.390353160049));
#26212=CARTESIAN_POINT('Ctrl Pts',(85.9522239607591,95.6236167989524,197.452797942955));
#26213=CARTESIAN_POINT('Ctrl Pts',(85.9853072081226,95.6340261702735,197.475575268837));
#26214=CARTESIAN_POINT('Ctrl Pts',(86.0381104013451,95.6628199399351,197.50541610126));
#26215=CARTESIAN_POINT('Ctrl Pts',(86.0599824910312,95.67909256943,197.51545301994));
#26216=CARTESIAN_POINT('Ctrl Pts',(86.0912442094499,95.7119965209056,197.524679726807));
#26217=CARTESIAN_POINT('Ctrl Pts',(86.1018504288941,95.7256648117306,197.526481344743));
#26218=CARTESIAN_POINT('Ctrl Pts',(86.1109957247841,95.7403933692308,197.526481344607));
#26219=CARTESIAN_POINT('',(86.1113791955527,95.741012961473,197.526481344607));
#26220=CARTESIAN_POINT('',(86.1113791955527,95.741012961473,197.526481344607));
#26221=CARTESIAN_POINT('',(86.3065605834827,96.0574060274146,207.276481344607));
#26222=CARTESIAN_POINT('Origin',(86.6766969576459,97.1335683214121,183.174071706053));
#26223=CARTESIAN_POINT('',(86.8936178810123,97.009289147751,197.526481344607));
#26224=CARTESIAN_POINT('',(86.7995649337003,97.3512916790481,197.276481344607));
#26225=CARTESIAN_POINT('Ctrl Pts',(86.8936178810123,97.0092891477511,197.526481344607));
#26226=CARTESIAN_POINT('Ctrl Pts',(86.8938783775809,97.0097438269587,197.526481344607));
#26227=CARTESIAN_POINT('Ctrl Pts',(86.8941375763002,97.0101995550636,197.526479697129));
#26228=CARTESIAN_POINT('Ctrl Pts',(86.9059119225634,97.0310539697099,197.526329043289));
#26229=CARTESIAN_POINT('Ctrl Pts',(86.914296385724,97.0525943485027,197.522897090167));
#26230=CARTESIAN_POINT('Ctrl Pts',(86.9257598377503,97.0997764576947,197.509425478113));
#26231=CARTESIAN_POINT('Ctrl Pts',(86.9276623879705,97.1246972156251,197.49872862438));
#26232=CARTESIAN_POINT('Ctrl Pts',(86.9243822484398,97.180003725259,197.468545557741));
#26233=CARTESIAN_POINT('Ctrl Pts',(86.9166406619662,97.2092432027731,197.447428878785));
#26234=CARTESIAN_POINT('Ctrl Pts',(86.8941169849787,97.259932057604,197.403006214921));
#26235=CARTESIAN_POINT('Ctrl Pts',(86.8794821770795,97.2819696349757,197.37953436841));
#26236=CARTESIAN_POINT('Ctrl Pts',(86.8446722048286,97.3206341661874,197.330483552621));
#26237=CARTESIAN_POINT('Ctrl Pts',(86.8240336652295,97.3372030242998,197.304533630732));
#26238=CARTESIAN_POINT('Ctrl Pts',(86.8008698123469,97.3505514194756,197.277971923767));
#26239=CARTESIAN_POINT('Ctrl Pts',(86.8002182010604,97.3509230202178,197.277226632397));
#26240=CARTESIAN_POINT('Ctrl Pts',(86.7995649337003,97.3512916790481,197.276481344607));
#26241=CARTESIAN_POINT('',(86.7995649337003,97.3512916790481,183.174071706053));
#26242=CARTESIAN_POINT('',(86.8894679405697,97.0023109070477,197.526481344607));
#26243=CARTESIAN_POINT('',(86.8894679405697,97.0023109070477,197.526481344607));
#26244=CARTESIAN_POINT('Origin',(86.6766969576459,97.1335683214121,197.526481344607));
#26245=CARTESIAN_POINT('Origin',(77.215862801455,80.368869783441,207.276481344607));
#26246=CARTESIAN_POINT('Origin',(77.215862801455,80.368869783441,207.526481344607));
#26247=CARTESIAN_POINT('Origin',(77.215862801455,80.368869783441,207.276481344607));
#26248=CARTESIAN_POINT('Origin',(66.0612008874025,94.6747068168279,207.276481344607));
#26249=CARTESIAN_POINT('',(65.8706178185259,94.512910358716,207.276481344607));
#26250=CARTESIAN_POINT('Origin',(66.0612008874025,94.6747068168279,207.276481344607));
#26251=CARTESIAN_POINT('Origin',(66.0612008874025,94.6747068168279,207.276481344607));
#26252=CARTESIAN_POINT('Origin',(77.215862801455,80.368869783441,197.276481344607));
#26253=CARTESIAN_POINT('',(87.0302049776637,94.8697252003878,197.285998170767));
#26254=CARTESIAN_POINT('',(86.9620814661663,95.2153625964141,197.526481344568));
#26255=CARTESIAN_POINT('Ctrl Pts',(87.0302047491998,94.8697253476385,197.285998010414));
#26256=CARTESIAN_POINT('Ctrl Pts',(87.0293873488746,94.8703254048265,197.287016105511));
#26257=CARTESIAN_POINT('Ctrl Pts',(87.0293554761683,94.8703809253921,197.287632834136));
#26258=CARTESIAN_POINT('Ctrl Pts',(87.0282421949799,94.8711981752271,197.288758182633));
#26259=CARTESIAN_POINT('Ctrl Pts',(87.0274485389422,94.8717814515778,197.289656234906));
#26260=CARTESIAN_POINT('Ctrl Pts',(87.0076896512662,94.8869284991216,197.313936094399));
#26261=CARTESIAN_POINT('Ctrl Pts',(86.9916554589569,94.9030932672712,197.336722197331));
#26262=CARTESIAN_POINT('Ctrl Pts',(86.9533411021071,94.953758427131,197.396368011346));
#26263=CARTESIAN_POINT('Ctrl Pts',(86.9367358693936,94.9912035179937,197.430388733357));
#26264=CARTESIAN_POINT('Ctrl Pts',(86.9232850558868,95.0616415164893,197.47902078915));
#26265=CARTESIAN_POINT('Ctrl Pts',(86.9229006039806,95.0928025207568,197.495729267709));
#26266=CARTESIAN_POINT('Ctrl Pts',(86.9318852326942,95.1474151109197,197.516701595193));
#26267=CARTESIAN_POINT('Ctrl Pts',(86.9394044252834,95.171765230652,197.523029647908));
#26268=CARTESIAN_POINT('Ctrl Pts',(86.9543584616972,95.2020873466914,197.526129019956));
#26269=CARTESIAN_POINT('Ctrl Pts',(86.9580752868692,95.2088258280812,197.5264813447));
#26270=CARTESIAN_POINT('Ctrl Pts',(86.9620814697059,95.2153625942447,197.526481344607));
#26271=CARTESIAN_POINT('Origin',(77.215862801455,80.368869783441,197.526481344607));
#26272=CARTESIAN_POINT('Origin',(77.215862801455,80.368869783441,197.285998250943));
#26273=CARTESIAN_POINT('Origin',(77.215862801455,80.368869783441,197.276481344607));
#26274=CARTESIAN_POINT('',(87.744926219196,96.4841210549909,197.526481344607));
#26275=CARTESIAN_POINT('',(88.0927703883544,96.553519342392,197.276481344607));
#26276=CARTESIAN_POINT('Ctrl Pts',(87.744926219196,96.4841210549908,197.526481344607));
#26277=CARTESIAN_POINT('Ctrl Pts',(87.7452156792141,96.4845578667829,197.526481344607));
#26278=CARTESIAN_POINT('Ctrl Pts',(87.745506658949,96.484993989329,197.526479697129));
#26279=CARTESIAN_POINT('Ctrl Pts',(87.7588610072407,96.5048737081865,197.526329043289));
#26280=CARTESIAN_POINT('Ctrl Pts',(87.7743493927896,96.5220317108126,197.522897090168));
#26281=CARTESIAN_POINT('Ctrl Pts',(87.8113719962568,96.5534465002068,197.509425478114));
#26282=CARTESIAN_POINT('Ctrl Pts',(87.8327897428621,96.5663284256653,197.49872862438));
#26283=CARTESIAN_POINT('Ctrl Pts',(87.8836882989136,96.5882123539018,197.468545557742));
#26284=CARTESIAN_POINT('Ctrl Pts',(87.9132928417027,96.5944131806742,197.447428878786));
#26285=CARTESIAN_POINT('Ctrl Pts',(87.9686989911511,96.5970274936707,197.403006214922));
#26286=CARTESIAN_POINT('Ctrl Pts',(87.9949601815994,96.5938365228299,197.379534368411));
#26287=CARTESIAN_POINT('Ctrl Pts',(88.0451330397623,96.580075547367,197.330483552623));
#26288=CARTESIAN_POINT('Ctrl Pts',(88.0692006987673,96.5690653627259,197.304533630731));
#26289=CARTESIAN_POINT('Ctrl Pts',(88.0915233437827,96.554353352199,197.27797192377));
#26290=CARTESIAN_POINT('Ctrl Pts',(88.0921478091168,96.5539377473013,197.277226632396));
#26291=CARTESIAN_POINT('Ctrl Pts',(88.0927703883544,96.5535193423919,197.276481344607));
#26292=CARTESIAN_POINT('Origin',(77.215862801455,80.368869783441,197.276481344607));
#26293=CARTESIAN_POINT('Origin',(77.215862801455,80.368869783441,197.526481344607));
#26294=CARTESIAN_POINT('Origin',(64.8042619416421,96.1552786690737,207.276481344607));
#26295=CARTESIAN_POINT('',(64.6136788727654,95.9934822109618,207.276481344607));
#26296=CARTESIAN_POINT('',(88.001300134864,68.8310542744068,207.526481344607));
#26297=CARTESIAN_POINT('Origin',(66.1853223820777,94.5285011270022,202.246481276341));
#26298=CARTESIAN_POINT('',(66.1112139395638,94.2295076956275,197.526481344607));
#26299=CARTESIAN_POINT('',(66.1112139395638,94.2295076956275,197.526481344607));
#26300=CARTESIAN_POINT('',(66.1116408285149,94.2290061991774,197.526481344578));
#26301=CARTESIAN_POINT('',(66.1116408097593,94.2290062155739,197.52648134452));
#26302=CARTESIAN_POINT('',(66.4614031347772,94.1868912572728,197.285998169697));
#26303=CARTESIAN_POINT('Ctrl Pts',(66.1116408313988,94.2290062016389,197.526481344607));
#26304=CARTESIAN_POINT('Ctrl Pts',(66.1169211525317,94.2228196133348,197.526481344688));
#26305=CARTESIAN_POINT('Ctrl Pts',(66.1225164472751,94.2168744591204,197.526084798852));
#26306=CARTESIAN_POINT('Ctrl Pts',(66.1472603113197,94.1930214631972,197.522744043761));
#26307=CARTESIAN_POINT('Ctrl Pts',(66.1682407124789,94.1784248076749,197.516246088138));
#26308=CARTESIAN_POINT('Ctrl Pts',(66.2177375812335,94.1532020157617,197.494874084349));
#26309=CARTESIAN_POINT('Ctrl Pts',(66.2477024906526,94.1440934241378,197.477895158506));
#26310=CARTESIAN_POINT('Ctrl Pts',(66.3192752562298,94.1356134414265,197.428597050384));
#26311=CARTESIAN_POINT('Ctrl Pts',(66.3601923972269,94.1402155954496,197.394186199542));
#26312=CARTESIAN_POINT('Ctrl Pts',(66.432503312338,94.1660665527557,197.32179389136));
#26313=CARTESIAN_POINT('Ctrl Pts',(66.454375282936,94.1820035053602,197.294649845323));
#26314=CARTESIAN_POINT('Ctrl Pts',(66.4584424176479,94.1848017482204,197.289840338499));
#26315=CARTESIAN_POINT('Ctrl Pts',(66.4593281118165,94.1854321505868,197.28882852111));
#26316=CARTESIAN_POINT('Ctrl Pts',(66.4605216743804,94.1862901108438,197.287634889492));
#26317=CARTESIAN_POINT('Ctrl Pts',(66.460580587625,94.186300146126,197.287014717403));
#26318=CARTESIAN_POINT('Ctrl Pts',(66.4614029209132,94.1868910829801,197.285998007206));
#26319=CARTESIAN_POINT('',(66.35154481532,94.3164511783277,201.74111193235));
#26320=CARTESIAN_POINT('Origin',(87.2697224402081,95.237894233865,202.246481277241));
#26321=CARTESIAN_POINT('',(87.1194741085686,95.0142415830358,201.741111932351));
#26322=CARTESIAN_POINT('',(86.9624631272481,95.2159833040156,197.526481344607));
#26323=CARTESIAN_POINT('',(86.9624631272481,95.2159833040156,197.526481344607));
#26324=CARTESIAN_POINT('',(86.9620814785655,95.2153626241862,197.526481344489));
#26325=CARTESIAN_POINT('Origin',(87.953322855189,96.3460238352259,183.174071706053));
#26326=CARTESIAN_POINT('',(87.7405518722651,96.4772812495903,207.276481344607));
#26327=CARTESIAN_POINT('',(88.0927703883544,96.553519342392,207.276481344607));
#26328=CARTESIAN_POINT('Origin',(87.953322855189,96.3460238352259,207.276481344607));
#26329=CARTESIAN_POINT('',(88.0927703883544,96.553519342392,183.174071706053));
#26330=CARTESIAN_POINT('',(87.7405518722651,96.4772812495903,197.526481344607));
#26331=CARTESIAN_POINT('Origin',(87.953322855189,96.3460238352259,197.526481344607));
#26332=CARTESIAN_POINT('',(87.7405518722651,96.4772812495903,197.526481344607));
#26333=CARTESIAN_POINT('Origin',(65.3426635064322,95.5210854135286,183.174071706053));
#26334=CARTESIAN_POINT('',(65.1520804375556,95.3592889554166,197.526481344607));
#26335=CARTESIAN_POINT('',(65.1468869158002,95.3656134657036,197.526481344607));
#26336=CARTESIAN_POINT('Origin',(65.3426635064322,95.5210854135286,197.526481344607));
#26337=CARTESIAN_POINT('',(65.1520804375556,95.3592889554166,197.526481344607));
#26338=CARTESIAN_POINT('',(65.1884661129904,95.7178674346986,197.276481344607));
#26339=CARTESIAN_POINT('',(65.1884661129904,95.7178674346986,183.174071706053));
#26340=CARTESIAN_POINT('Ctrl Pts',(65.1884661129904,95.7178674346985,197.276481344607));
#26341=CARTESIAN_POINT('Ctrl Pts',(65.1878756789987,95.7174047736182,197.277226632395));
#26342=CARTESIAN_POINT('Ctrl Pts',(65.1872873244521,95.7169394529637,197.277971923769));
#26343=CARTESIAN_POINT('Ctrl Pts',(65.1663929788226,95.7002610221315,197.304533630727));
#26344=CARTESIAN_POINT('Ctrl Pts',(65.1484793144624,95.6807782860578,197.330483552621));
#26345=CARTESIAN_POINT('Ctrl Pts',(65.1198763396659,95.6373208358935,197.37953436841));
#26346=CARTESIAN_POINT('Ctrl Pts',(65.1087201860209,95.6133339091515,197.403006214922));
#26347=CARTESIAN_POINT('Ctrl Pts',(65.0940712628922,95.5598354504791,197.447428878785));
#26348=CARTESIAN_POINT('Ctrl Pts',(65.0908125131871,95.5297645383416,197.468545557742));
#26349=CARTESIAN_POINT('Ctrl Pts',(65.0958825740711,95.4745933157176,197.49872862438));
#26350=CARTESIAN_POINT('Ctrl Pts',(65.1015092658451,95.4502416378935,197.509425478113));
#26351=CARTESIAN_POINT('Ctrl Pts',(65.1199342711905,95.4053185776885,197.522897090168));
#26352=CARTESIAN_POINT('Ctrl Pts',(65.131461144181,95.3852831505632,197.526329043289));
#26353=CARTESIAN_POINT('Ctrl Pts',(65.1462362842778,95.3664354166072,197.526479697129));
#26354=CARTESIAN_POINT('Ctrl Pts',(65.1465610373146,95.3660238251271,197.526481344607));
#26355=CARTESIAN_POINT('Ctrl Pts',(65.1468869158002,95.3656134657036,197.526481344607));
#26356=CARTESIAN_POINT('Origin',(77.215862801455,80.368869783441,197.276481344607));
#26357=CARTESIAN_POINT('',(65.3491255130522,93.5820326593704,197.526481344555));
#26358=CARTESIAN_POINT('',(65.3337218174719,93.230084572225,197.285998194441));
#26359=CARTESIAN_POINT('Ctrl Pts',(65.3491255125137,93.5820326589161,197.526481344607));
#26360=CARTESIAN_POINT('Ctrl Pts',(65.3602746962636,93.5688145431561,197.526481344716));
#26361=CARTESIAN_POINT('Ctrl Pts',(65.36997193769,93.554539724584,197.524688976763));
#26362=CARTESIAN_POINT('Ctrl Pts',(65.39158902819,93.5146913614094,197.515495497821));
#26363=CARTESIAN_POINT('Ctrl Pts',(65.4003109763584,93.4888725096656,197.505476486175));
#26364=CARTESIAN_POINT('Ctrl Pts',(65.4113928007713,93.4297827815416,197.475678704812));
#26365=CARTESIAN_POINT('Ctrl Pts',(65.4110836642222,93.3951188265962,197.452930521194));
#26366=CARTESIAN_POINT('Ctrl Pts',(65.3952406789993,93.3179425315011,197.390550112667));
#26367=CARTESIAN_POINT('Ctrl Pts',(65.3755108879767,93.2775983899897,197.349058772659));
#26368=CARTESIAN_POINT('Ctrl Pts',(65.341353172853,93.2378215388855,197.296918842359));
#26369=CARTESIAN_POINT('Ctrl Pts',(65.3368138008746,93.2332094505631,197.290407199789));
#26370=CARTESIAN_POINT('Ctrl Pts',(65.3346982702197,93.2310710756822,197.287528959007));
#26371=CARTESIAN_POINT('Ctrl Pts',(65.3344917686414,93.2308525241048,197.287089779763));
#26372=CARTESIAN_POINT('Ctrl Pts',(65.3337219804242,93.2300847198161,197.285998137443));
#26373=CARTESIAN_POINT('Origin',(77.215862801455,80.368869783441,197.285998250943));
#26374=CARTESIAN_POINT('Origin',(77.215862801455,80.368869783441,197.526481344607));
#26375=CARTESIAN_POINT('Origin',(87.953322855189,96.3460238352259,207.276481344607));
#26376=CARTESIAN_POINT('',(87.953322855189,96.3460238352259,207.526481344607));
#26377=CARTESIAN_POINT('Origin',(87.953322855189,96.3460238352259,207.276481344607));
#26378=CARTESIAN_POINT('Origin',(87.953322855189,96.3460238352259,207.276481344607));
#26379=CARTESIAN_POINT('Origin',(77.215862801455,80.368869783441,197.276481344607));
#26380=CARTESIAN_POINT('',(64.3841861492998,94.7184542476175,197.526481344607));
#26381=CARTESIAN_POINT('Origin',(77.215862801455,80.368869783441,197.526481344607));
#26382=CARTESIAN_POINT('',(64.0298626660881,94.7347808380907,197.276481344607));
#26383=CARTESIAN_POINT('Origin',(77.215862801455,80.368869783441,197.276481344607));
#26384=CARTESIAN_POINT('Ctrl Pts',(64.0298626660881,94.7347808380907,197.276481344607));
#26385=CARTESIAN_POINT('Ctrl Pts',(64.0304152834259,94.73528806748,197.277226632396));
#26386=CARTESIAN_POINT('Ctrl Pts',(64.030970186294,94.7357928121606,197.277971923767));
#26387=CARTESIAN_POINT('Ctrl Pts',(64.050827920147,94.7536929277923,197.304533630741));
#26388=CARTESIAN_POINT('Ctrl Pts',(64.0729672526987,94.7681955596412,197.330483552619));
#26389=CARTESIAN_POINT('Ctrl Pts',(64.1205017521378,94.7893415168146,197.379534368405));
#26390=CARTESIAN_POINT('Ctrl Pts',(64.1459849761886,94.796443467996,197.403006214916));
#26391=CARTESIAN_POINT('Ctrl Pts',(64.2011546284904,94.8021867679137,197.44742887878));
#26392=CARTESIAN_POINT('Ctrl Pts',(64.2313548721284,94.8005061458102,197.468545557738));
#26393=CARTESIAN_POINT('Ctrl Pts',(64.2849644912409,94.7865212231472,197.498728624377));
#26394=CARTESIAN_POINT('Ctrl Pts',(64.3080751589899,94.7770048735645,197.509425478111));
#26395=CARTESIAN_POINT('Ctrl Pts',(64.3493990161624,94.7515117178442,197.522897090166));
#26396=CARTESIAN_POINT('Ctrl Pts',(64.3672904066541,94.7368766473865,197.526329043289));
#26397=CARTESIAN_POINT('Ctrl Pts',(64.3834810958367,94.7192300209656,197.526479697129));
#26398=CARTESIAN_POINT('Ctrl Pts',(64.383834321995,94.7188425892111,197.526481344607));
#26399=CARTESIAN_POINT('Ctrl Pts',(64.3841861492998,94.7184542476174,197.526481344607));
#26400=CARTESIAN_POINT('Origin',(65.0415552428384,93.5580402355824,202.246481278135));
#26401=CARTESIAN_POINT('',(65.3337216550388,93.2300844250878,197.285998250943));
#26402=CARTESIAN_POINT('',(65.3486095562104,93.5826423840931,197.526481344607));
#26403=CARTESIAN_POINT('',(65.3486095562104,93.5826423840931,197.526481344607));
#26404=CARTESIAN_POINT('',(65.1080190161996,93.8660384731857,207.276481344607));
#26405=CARTESIAN_POINT('Origin',(77.215862801455,80.368869783441,207.276481344607));
#26406=CARTESIAN_POINT('',(95.0048109024016,76.8140447378918,207.526481344607));
#26407=CARTESIAN_POINT('Origin',(95.0048109024016,76.8140447378918,207.276481344607));
#26408=CARTESIAN_POINT('Origin',(77.215862801455,80.368869783441,207.526481344607));
#26409=CARTESIAN_POINT('Origin',(88.3891501308591,97.0525088614501,207.276481344607));
#26410=CARTESIAN_POINT('',(81.0179159409774,85.1035858117482,207.526481344607));
#26411=CARTESIAN_POINT('',(88.1763791479352,97.1837662758145,207.276481344607));
#26412=CARTESIAN_POINT('Origin',(77.215862801455,80.368869783441,207.276481344607));
#26413=CARTESIAN_POINT('Origin',(77.215862801455,80.368869783441,207.276481344607));
#26414=CARTESIAN_POINT('Origin',(77.215862801455,80.368869783441,207.526481344607));
#26415=CARTESIAN_POINT('Origin',(64.1989139498749,94.5506024912362,183.174071706053));
#26416=CARTESIAN_POINT('',(64.0298626660881,94.7347808380907,207.276481344607));
#26417=CARTESIAN_POINT('',(64.3894970187515,94.7123989493481,207.276481344607));
#26418=CARTESIAN_POINT('Origin',(64.1989139498749,94.5506024912362,207.276481344607));
#26419=CARTESIAN_POINT('',(64.3894970187515,94.7123989493481,197.526481344607));
#26420=CARTESIAN_POINT('',(64.3894970187515,94.7123989493481,197.526481344607));
#26421=CARTESIAN_POINT('Origin',(64.1989139498749,94.5506024912362,197.526481344607));
#26422=CARTESIAN_POINT('',(64.0298626660881,94.7347808380907,183.174071706053));
#26423=CARTESIAN_POINT('Origin',(95.0048109024016,76.8140447378918,207.276481344607));
#26424=CARTESIAN_POINT('',(94.9457275327917,76.5711267364272,207.276481344607));
#26425=CARTESIAN_POINT('Origin',(95.0048109024016,76.8140447378918,207.276481344607));
#26426=CARTESIAN_POINT('Origin',(95.0048109024016,76.8140447378918,207.276481344607));
#26427=CARTESIAN_POINT('Origin',(64.1989139498749,94.5506024912362,207.276481344607));
#26428=CARTESIAN_POINT('',(64.1989139498749,94.5506024912362,207.526481344607));
#26429=CARTESIAN_POINT('Origin',(64.1989139498749,94.5506024912362,207.276481344607));
#26430=CARTESIAN_POINT('Origin',(64.1989139498749,94.5506024912362,207.276481344607));
#26431=CARTESIAN_POINT('Origin',(63.719093831661,95.1157915670977,207.276481344607));
#26432=CARTESIAN_POINT('',(86.8578017216042,67.8602755257353,207.526481344607));
#26433=CARTESIAN_POINT('',(63.9096769005376,95.2775880252097,207.276481344607));
#26434=CARTESIAN_POINT('Origin',(77.215862801455,80.368869783441,207.276481344607));
#26435=CARTESIAN_POINT('Origin',(77.215862801455,80.368869783441,207.526481344607));
#26436=CARTESIAN_POINT('Origin',(94.8184588991746,76.8593694837389,202.246481277241));
#26437=CARTESIAN_POINT('',(94.3893078434365,76.95289179822,197.285998193683));
#26438=CARTESIAN_POINT('',(94.389307888928,76.9528920157415,197.285998250943));
#26439=CARTESIAN_POINT('',(94.5837977134794,76.6591576701982,197.526481344568));
#26440=CARTESIAN_POINT('Ctrl Pts',(94.3893077977898,76.9528915800162,197.285998135919));
#26441=CARTESIAN_POINT('Ctrl Pts',(94.3891366830531,76.9518182233094,197.287089433018));
#26442=CARTESIAN_POINT('Ctrl Pts',(94.3890984083501,76.9515210657439,197.287529424903));
#26443=CARTESIAN_POINT('Ctrl Pts',(94.3886471375595,76.9485644021981,197.290389360712));
#26444=CARTESIAN_POINT('Ctrl Pts',(94.3877023133716,76.9422601127003,197.296803640722));
#26445=CARTESIAN_POINT('Ctrl Pts',(94.3834217828299,76.8901250153594,197.348830521281));
#26446=CARTESIAN_POINT('Ctrl Pts',(94.3911493204423,76.8458687886726,197.390353067837));
#26447=CARTESIAN_POINT('Ctrl Pts',(94.423673374515,76.7740727220947,197.45279788084));
#26448=CARTESIAN_POINT('Ctrl Pts',(94.4437965561254,76.7458253439581,197.475575220366));
#26449=CARTESIAN_POINT('Ctrl Pts',(94.4874981390143,76.7045042673687,197.505416072974));
#26450=CARTESIAN_POINT('Ctrl Pts',(94.5097331760758,76.6887311845888,197.51545300005));
#26451=CARTESIAN_POINT('Ctrl Pts',(94.5506871134101,76.6691673834714,197.524679722475));
#26452=CARTESIAN_POINT('Ctrl Pts',(94.5669639509563,76.6633039945062,197.526481344743));
#26453=CARTESIAN_POINT('Ctrl Pts',(94.5837977136375,76.6591576708401,197.526481344607));
#26454=CARTESIAN_POINT('',(94.5845054798612,76.6589844329993,197.526481344607));
#26455=CARTESIAN_POINT('',(94.5845054798612,76.6589844329993,197.526481344607));
#26456=CARTESIAN_POINT('',(94.9457275327917,76.5711267364272,207.276481344607));
#26457=CARTESIAN_POINT('Origin',(96.4901086410159,76.4527854045269,207.276481344607));
#26458=CARTESIAN_POINT('',(96.4310252714059,76.2098674030624,207.276481344607));
#26459=CARTESIAN_POINT('',(96.3407170245198,76.4891209582564,207.526481344607));
#26460=CARTESIAN_POINT('Origin',(96.0835971249419,76.5516585634122,183.174071706053));
#26461=CARTESIAN_POINT('',(96.0324328587475,76.3069501290158,197.526481344607));
#26462=CARTESIAN_POINT('',(96.3286326356366,76.5020843917236,197.276481344607));
#26463=CARTESIAN_POINT('Ctrl Pts',(96.0324328587475,76.3069501290157,197.526481344607));
#26464=CARTESIAN_POINT('Ctrl Pts',(96.0329457822375,76.3068428856588,197.526481344607));
#26465=CARTESIAN_POINT('Ctrl Pts',(96.0334593022307,76.306737200757,197.526479697129));
#26466=CARTESIAN_POINT('Ctrl Pts',(96.0569315022667,76.3019835005518,197.526329043289));
#26467=CARTESIAN_POINT('Ctrl Pts',(96.0800085614862,76.3006657453395,197.522897090167));
#26468=CARTESIAN_POINT('Ctrl Pts',(96.1284238153765,76.3043434281616,197.509425478113));
#26469=CARTESIAN_POINT('Ctrl Pts',(96.1527127849481,76.3102349330904,197.498728624379));
#26470=CARTESIAN_POINT('Ctrl Pts',(96.2042987824697,76.3304451825418,197.468545557741));
#26471=CARTESIAN_POINT('Ctrl Pts',(96.2297148963087,76.3468433642625,197.447428878784));
#26472=CARTESIAN_POINT('Ctrl Pts',(96.2709626630343,76.3839283716008,197.403006214921));
#26473=CARTESIAN_POINT('Ctrl Pts',(96.2873992402467,76.4046568869407,197.379534368409));
#26474=CARTESIAN_POINT('Ctrl Pts',(96.3134145216056,76.4497111351057,197.330483552621));
#26475=CARTESIAN_POINT('Ctrl Pts',(96.3227947826065,76.4744596114168,197.304533630737));
#26476=CARTESIAN_POINT('Ctrl Pts',(96.3283318366233,76.5006146255939,197.277971923768));
#26477=CARTESIAN_POINT('Ctrl Pts',(96.3284838909699,76.5013491757008,197.277226632396));
#26478=CARTESIAN_POINT('Ctrl Pts',(96.3286326356366,76.5020843917236,197.276481344607));
#26479=CARTESIAN_POINT('',(96.3286326356366,76.5020843917236,183.174071706053));
#26480=CARTESIAN_POINT('',(96.0245137553319,76.3087405619477,197.526481344607));
#26481=CARTESIAN_POINT('',(96.0245137553319,76.3087405619477,197.526481344607));
#26482=CARTESIAN_POINT('Origin',(96.0835971249419,76.5516585634122,197.526481344607));
#26483=CARTESIAN_POINT('Origin',(77.215862801455,80.368869783441,207.276481344607));
#26484=CARTESIAN_POINT('',(58.9003582657663,73.6761652775505,207.276481344607));
#26485=CARTESIAN_POINT('',(59.1351724264803,73.7619691814722,207.526481344607));
#26486=CARTESIAN_POINT('Origin',(59.1351724264803,73.7619691814722,207.276481344607));
#26487=CARTESIAN_POINT('Origin',(77.215862801455,80.368869783441,207.526481344607));
#26488=CARTESIAN_POINT('Origin',(77.215862801455,80.368869783441,207.276481344607));
#26489=CARTESIAN_POINT('Origin',(77.215862801455,80.368869783441,197.276481344607));
#26490=CARTESIAN_POINT('',(94.0397943586528,75.5158864604089,197.285998170767));
#26491=CARTESIAN_POINT('',(94.3474637336519,75.6874835992026,197.526481344568));
#26492=CARTESIAN_POINT('Ctrl Pts',(94.0397944280951,75.5158867231863,197.285998010414));
#26493=CARTESIAN_POINT('Ctrl Pts',(94.0401125259821,75.5168495455053,197.287016106087));
#26494=CARTESIAN_POINT('Ctrl Pts',(94.0401554804701,75.5168970170074,197.287632833281));
#26495=CARTESIAN_POINT('Ctrl Pts',(94.0405887095143,75.518208357421,197.288758185983));
#26496=CARTESIAN_POINT('Ctrl Pts',(94.0408981874299,75.5191434185213,197.289656246106));
#26497=CARTESIAN_POINT('Ctrl Pts',(94.0491981798594,75.54261627962,197.313936475957));
#26498=CARTESIAN_POINT('Ctrl Pts',(94.0596171630581,75.5628612000245,197.336722933864));
#26499=CARTESIAN_POINT('Ctrl Pts',(94.095963205002,75.6149568033014,197.396368929828));
#26500=CARTESIAN_POINT('Ctrl Pts',(94.1264443408684,75.6423203109527,197.430389486829));
#26501=CARTESIAN_POINT('Ctrl Pts',(94.189278308267,75.6768790524282,197.479021261726));
#26502=CARTESIAN_POINT('Ctrl Pts',(94.2187953499103,75.6868738596624,197.49572962646));
#26503=CARTESIAN_POINT('Ctrl Pts',(94.273511348843,75.6952050320096,197.516701785659));
#26504=CARTESIAN_POINT('Ctrl Pts',(94.2989932171594,75.6955783896931,197.52302976678));
#26505=CARTESIAN_POINT('Ctrl Pts',(94.3324520692234,75.6907262606351,197.526129038087));
#26506=CARTESIAN_POINT('Ctrl Pts',(94.3400091118565,75.6892736835662,197.5264813447));
#26507=CARTESIAN_POINT('Ctrl Pts',(94.3474637326825,75.6874835951658,197.526481344607));
#26508=CARTESIAN_POINT('Origin',(77.215862801455,80.368869783441,197.526481344607));
#26509=CARTESIAN_POINT('Origin',(77.215862801455,80.368869783441,197.285998250943));
#26510=CARTESIAN_POINT('Origin',(77.215862801455,80.368869783441,197.276481344607));
#26511=CARTESIAN_POINT('',(95.7960370659294,75.3350219210433,197.526481344607));
#26512=CARTESIAN_POINT('',(95.969528519046,75.0256477074975,197.276481344607));
#26513=CARTESIAN_POINT('Ctrl Pts',(95.7960370659294,75.3350219210434,197.526481344607));
#26514=CARTESIAN_POINT('Ctrl Pts',(95.7965419466967,75.3348816104736,197.526481344607));
#26515=CARTESIAN_POINT('Ctrl Pts',(95.7970466415705,75.3347396415787,197.526479697129));
#26516=CARTESIAN_POINT('Ctrl Pts',(95.8200800983042,75.3281820725845,197.526329043289));
#26517=CARTESIAN_POINT('Ctrl Pts',(95.8411845028582,75.3187538569821,197.522897090167));
#26518=CARTESIAN_POINT('Ctrl Pts',(95.8825023566668,75.2932509725011,197.509425478112));
#26519=CARTESIAN_POINT('Ctrl Pts',(95.9013722434987,75.2768622189142,197.498728624378));
#26520=CARTESIAN_POINT('Ctrl Pts',(95.9379136148588,75.235217321239,197.468545557739));
#26521=CARTESIAN_POINT('Ctrl Pts',(95.9529592583993,75.2089778887585,197.447428878781));
#26522=CARTESIAN_POINT('Ctrl Pts',(95.972567059581,75.1570913764279,197.403006214918));
#26523=CARTESIAN_POINT('Ctrl Pts',(95.97764742011,75.1311294359093,197.379534368408));
#26524=CARTESIAN_POINT('Ctrl Pts',(95.9800642205536,75.0791598369372,197.330483552621));
#26525=CARTESIAN_POINT('Ctrl Pts',(95.9770302283516,75.0528677988418,197.304533630734));
#26526=CARTESIAN_POINT('Ctrl Pts',(95.9699363515425,75.0270914405678,197.277971923769));
#26527=CARTESIAN_POINT('Ctrl Pts',(95.9697340581972,75.026369109767,197.277226632397));
#26528=CARTESIAN_POINT('Ctrl Pts',(95.9695285190461,75.0256477074975,197.276481344607));
#26529=CARTESIAN_POINT('Origin',(77.215862801455,80.368869783441,197.276481344607));
#26530=CARTESIAN_POINT('Origin',(77.215862801455,80.368869783441,197.526481344607));
#26531=CARTESIAN_POINT('Origin',(59.1351724264803,73.7619691814722,207.276481344607));
#26532=CARTESIAN_POINT('',(59.2301565951581,73.5307160567353,207.276481344607));
#26533=CARTESIAN_POINT('Origin',(59.1351724264803,73.7619691814722,207.276481344607));
#26534=CARTESIAN_POINT('Origin',(59.1351724264803,73.7619691814722,207.276481344607));
#26535=CARTESIAN_POINT('Origin',(58.3694473018174,73.4474576933157,207.276481344607));
#26536=CARTESIAN_POINT('',(58.4644314704952,73.2162045685788,207.276481344607));
#26537=CARTESIAN_POINT('',(91.5206923608871,87.0638940383495,207.526481344607));
#26538=CARTESIAN_POINT('Origin',(60.3395802182522,74.2566633166929,202.246481275782));
#26539=CARTESIAN_POINT('',(60.6010403165656,74.0937884510217,197.526481344607));
#26540=CARTESIAN_POINT('',(60.6010403165656,74.0937884510217,197.526481344607));
#26541=CARTESIAN_POINT('',(60.6016091647915,74.0940229189345,197.526481344583));
#26542=CARTESIAN_POINT('',(60.6016091462116,74.09402290755,197.526481344536));
#26543=CARTESIAN_POINT('',(60.7498001670302,74.4136282692967,197.285998169033));
#26544=CARTESIAN_POINT('Ctrl Pts',(60.601609163429,74.0940229222286,197.526481344607));
#26545=CARTESIAN_POINT('Ctrl Pts',(60.6093867240074,74.0972399164823,197.526481344681));
#26546=CARTESIAN_POINT('Ctrl Pts',(60.6170211752848,74.1008569650917,197.526056720543));
#26547=CARTESIAN_POINT('Ctrl Pts',(60.6476006570278,74.1172759128502,197.522566777863));
#26548=CARTESIAN_POINT('Ctrl Pts',(60.6679478441437,74.1328180135862,197.515965357168));
#26549=CARTESIAN_POINT('Ctrl Pts',(60.7071790802335,74.1723286486342,197.494349617611));
#26550=CARTESIAN_POINT('Ctrl Pts',(60.7250505559069,74.1981631566551,197.477205674158));
#26551=CARTESIAN_POINT('Ctrl Pts',(60.7550237921088,74.2639499490842,197.427502643351));
#26552=CARTESIAN_POINT('Ctrl Pts',(60.7631014541665,74.304456312216,197.392855833564));
#26553=CARTESIAN_POINT('Ctrl Pts',(60.7604399586737,74.379903994817,197.321521323378));
#26554=CARTESIAN_POINT('Ctrl Pts',(60.7524970087799,74.4046892292434,197.295405117688));
#26555=CARTESIAN_POINT('Ctrl Pts',(60.7508644926709,74.4101900577452,197.289818721891));
#26556=CARTESIAN_POINT('Ctrl Pts',(60.750542989354,74.411213629704,197.288821964585));
#26557=CARTESIAN_POINT('Ctrl Pts',(60.7500979523006,74.4126077588179,197.287636169735));
#26558=CARTESIAN_POINT('Ctrl Pts',(60.7501077413797,74.412664072175,197.287013854275));
#26559=CARTESIAN_POINT('Ctrl Pts',(60.7498002675722,74.4136280096502,197.285998005213));
#26560=CARTESIAN_POINT('',(60.5926319977064,74.3491829380803,201.741111932353));
#26561=CARTESIAN_POINT('Origin',(94.4639588834092,75.4018623050297,202.246481277241));
#26562=CARTESIAN_POINT('',(94.2048232846065,75.4756444899691,201.741111932351));
#26563=CARTESIAN_POINT('',(94.7093940543517,75.599454730569,207.276481344607));
#26564=CARTESIAN_POINT('Origin',(94.6503106847418,75.3565367291045,207.276481344607));
#26565=CARTESIAN_POINT('',(94.3481720014213,75.6873124271411,197.526481344607));
#26566=CARTESIAN_POINT('',(94.3481720014213,75.6873124271411,197.526481344607));
#26567=CARTESIAN_POINT('',(94.3474637638963,75.6874835959923,197.526481344489));
#26568=CARTESIAN_POINT('Origin',(95.7290969072821,75.0941505546249,183.174071706053));
#26569=CARTESIAN_POINT('',(95.969528519046,75.0256477074975,183.174071706053));
#26570=CARTESIAN_POINT('',(95.788180276892,75.3370685560895,197.526481344607));
#26571=CARTESIAN_POINT('Origin',(95.7290969072821,75.0941505546249,197.526481344607));
#26572=CARTESIAN_POINT('',(95.788180276892,75.3370685560895,197.526481344607));
#26573=CARTESIAN_POINT('Origin',(59.1351724264803,73.7619691814722,183.174071706053));
#26574=CARTESIAN_POINT('',(59.2301565951581,73.5307160567353,197.526481344607));
#26575=CARTESIAN_POINT('',(59.2224992886726,73.5277171395608,197.526481344607));
#26576=CARTESIAN_POINT('Origin',(59.1351724264803,73.7619691814722,197.526481344607));
#26577=CARTESIAN_POINT('',(59.2301565951581,73.5307160567353,197.526481344607));
#26578=CARTESIAN_POINT('',(58.9003582657663,73.6761652775505,197.276481344607));
#26579=CARTESIAN_POINT('',(58.9003582657663,73.6761652775505,183.174071706053));
#26580=CARTESIAN_POINT('Ctrl Pts',(58.9003582657663,73.6761652775505,197.276481344607));
#26581=CARTESIAN_POINT('Ctrl Pts',(58.9006157158184,73.6754607301448,197.277226632397));
#26582=CARTESIAN_POINT('Ctrl Pts',(58.9008763380428,73.6747573380522,197.277971923768));
#26583=CARTESIAN_POINT('Ctrl Pts',(58.9102777590331,73.649730212411,197.304533630725));
#26584=CARTESIAN_POINT('Ctrl Pts',(58.9232676286132,73.6266707314127,197.330483552622));
#26585=CARTESIAN_POINT('Ctrl Pts',(58.9557528174119,73.5860334006603,197.37953436841));
#26586=CARTESIAN_POINT('Ctrl Pts',(58.9751154174747,73.5680078039303,197.403006214922));
#26587=CARTESIAN_POINT('Ctrl Pts',(59.0214638375681,73.5375365062228,197.447428878785));
#26588=CARTESIAN_POINT('Ctrl Pts',(59.0490539838186,73.525140416666,197.468545557742));
#26589=CARTESIAN_POINT('Ctrl Pts',(59.1030897139364,73.5129048458243,197.49872862438));
#26590=CARTESIAN_POINT('Ctrl Pts',(59.1279879313116,73.5107270844252,197.509425478113));
#26591=CARTESIAN_POINT('Ctrl Pts',(59.1764065218,73.5143605752103,197.522897090168));
#26592=CARTESIAN_POINT('Ctrl Pts',(59.1990241075803,73.5191283791597,197.526329043289));
#26593=CARTESIAN_POINT('Ctrl Pts',(59.2215164523983,73.5273525061497,197.526479697129));
#26594=CARTESIAN_POINT('Ctrl Pts',(59.2220082824058,73.5275340972434,197.526481344607));
#26595=CARTESIAN_POINT('Ctrl Pts',(59.2224992886726,73.5277171395608,197.526481344607));
#26596=CARTESIAN_POINT('Origin',(77.215862801455,80.368869783441,197.276481344607));
#26597=CARTESIAN_POINT('',(60.981127142278,73.168836093202,197.526481344546));
#26598=CARTESIAN_POINT('',(61.3110675966908,73.045372688363,197.285998194906));
#26599=CARTESIAN_POINT('Ctrl Pts',(60.9811271425581,73.1688360925134,197.526481344607));
#26600=CARTESIAN_POINT('Ctrl Pts',(60.9971187919203,73.1753416507812,197.526481344728));
#26601=CARTESIAN_POINT('Ctrl Pts',(61.0136652535945,73.180145472812,197.524694774696));
#26602=CARTESIAN_POINT('Ctrl Pts',(61.0582096361667,73.1883912015722,197.515522145646));
#26603=CARTESIAN_POINT('Ctrl Pts',(61.0854542226308,73.1887128146243,197.5055143784));
#26604=CARTESIAN_POINT('Ctrl Pts',(61.1450631440005,73.1810065035281,197.475743629358));
#26605=CARTESIAN_POINT('Ctrl Pts',(61.1779277820307,73.1700125943206,197.453013745431));
#26606=CARTESIAN_POINT('Ctrl Pts',(61.2464250100863,73.1311281924925,197.390673688517));
#26607=CARTESIAN_POINT('Ctrl Pts',(61.2787026839839,73.0999163692651,197.34920192024));
#26608=CARTESIAN_POINT('Ctrl Pts',(61.3060362721128,73.0550865202932,197.296991136723));
#26609=CARTESIAN_POINT('Ctrl Pts',(61.3090465299422,73.0492895571933,197.290418308859));
#26610=CARTESIAN_POINT('Ctrl Pts',(61.310430982896,73.0466070939639,197.287528672697));
#26611=CARTESIAN_POINT('Ctrl Pts',(61.3105752351829,73.0463425312112,197.287089992911));
#26612=CARTESIAN_POINT('Ctrl Pts',(61.3110675074857,73.0453728872428,197.28599813838));
#26613=CARTESIAN_POINT('Origin',(77.215862801455,80.368869783441,197.285998250943));
#26614=CARTESIAN_POINT('Origin',(77.215862801455,80.368869783441,197.526481344607));
#26615=CARTESIAN_POINT('Origin',(94.6503106847418,75.3565367291045,207.276481344607));
#26616=CARTESIAN_POINT('',(94.6503106847418,75.3565367291045,207.526481344607));
#26617=CARTESIAN_POINT('Origin',(94.6503106847418,75.3565367291045,207.276481344607));
#26618=CARTESIAN_POINT('Origin',(94.6503106847418,75.3565367291045,207.276481344607));
#26619=CARTESIAN_POINT('Origin',(77.215862801455,80.368869783441,197.276481344607));
#26620=CARTESIAN_POINT('',(59.602148855249,72.6023016210397,197.526481344607));
#26621=CARTESIAN_POINT('Origin',(77.215862801455,80.368869783441,197.526481344607));
#26622=CARTESIAN_POINT('',(59.4770762970785,72.2703851503661,197.276481344607));
#26623=CARTESIAN_POINT('Origin',(77.215862801455,80.368869783441,197.276481344607));
#26624=CARTESIAN_POINT('Ctrl Pts',(59.4770762970785,72.2703851503661,197.276481344607));
#26625=CARTESIAN_POINT('Ctrl Pts',(59.4767647705069,72.2710675130049,197.277226632396));
#26626=CARTESIAN_POINT('Ctrl Pts',(59.4764563135271,72.2717512810019,197.277971923768));
#26627=CARTESIAN_POINT('Ctrl Pts',(59.4655725732334,72.2961702885867,197.304533630729));
#26628=CARTESIAN_POINT('Ctrl Pts',(59.4586252638423,72.3217087158688,197.330483552621));
#26629=CARTESIAN_POINT('Ctrl Pts',(59.453211504542,72.3734520376809,197.379534368409));
#26630=CARTESIAN_POINT('Ctrl Pts',(59.4543361227423,72.3998824681079,197.403006214921));
#26631=CARTESIAN_POINT('Ctrl Pts',(59.4659309527633,72.4541248495629,197.447428878784));
#26632=CARTESIAN_POINT('Ctrl Pts',(59.4768662169522,72.4823258992516,197.468545557741));
#26633=CARTESIAN_POINT('Ctrl Pts',(59.5067404126769,72.5289853222335,197.498728624379));
#26634=CARTESIAN_POINT('Ctrl Pts',(59.5229356318641,72.5480215705154,197.509425478113));
#26635=CARTESIAN_POINT('Ctrl Pts',(59.5599558615497,72.5794391572182,197.522897090167));
#26636=CARTESIAN_POINT('Ctrl Pts',(59.5794053816239,72.5919292857166,197.526329043289));
#26637=CARTESIAN_POINT('Ctrl Pts',(59.6011931085822,72.6018709553029,197.526479697129));
#26638=CARTESIAN_POINT('Ctrl Pts',(59.6016707655249,72.6020870939782,197.526481344607));
#26639=CARTESIAN_POINT('Ctrl Pts',(59.602148855249,72.6023016210397,197.526481344607));
#26640=CARTESIAN_POINT('Origin',(60.9088619358641,72.8688894817693,202.246481278685));
#26641=CARTESIAN_POINT('',(60.6364778870401,73.0272774920494,207.276481344607));
#26642=CARTESIAN_POINT('Origin',(60.7314620557179,72.7960243673124,207.276481344607));
#26643=CARTESIAN_POINT('',(61.3110676856272,73.0453724901115,197.285998250943));
#26644=CARTESIAN_POINT('',(60.9803477063441,73.1685174815939,197.526481344607));
#26645=CARTESIAN_POINT('',(60.9803477063441,73.1685174815939,197.526481344607));
#26646=CARTESIAN_POINT('',(60.6364778870401,73.0272774920494,207.276481344607));
#26647=CARTESIAN_POINT('Origin',(77.215862801455,80.368869783441,207.276481344607));
#26648=CARTESIAN_POINT('Origin',(77.215862801455,80.368869783441,207.526481344607));
#26649=CARTESIAN_POINT('Origin',(96.135608423356,74.9952773957396,207.276481344607));
#26650=CARTESIAN_POINT('',(95.9862168068599,75.0316129494691,207.526481344607));
#26651=CARTESIAN_POINT('',(96.194691792966,75.2381953972042,207.276481344607));
#26652=CARTESIAN_POINT('Origin',(77.215862801455,80.368869783441,207.276481344607));
#26653=CARTESIAN_POINT('',(79.4109822996944,61.2444364483471,207.526481344607));
#26654=CARTESIAN_POINT('',(79.4394903451261,60.996067184255,207.276481344607));
#26655=CARTESIAN_POINT('Origin',(79.4109822996944,61.2444364483471,207.276481344607));
#26656=CARTESIAN_POINT('Origin',(77.215862801455,80.368869783441,207.276481344607));
#26657=CARTESIAN_POINT('Origin',(77.215862801455,80.368869783441,207.526481344607));
#26658=CARTESIAN_POINT('Origin',(59.7044966368782,72.3742118764312,183.174071706053));
#26659=CARTESIAN_POINT('',(59.6095124682004,72.6054650011681,197.526481344607));
#26660=CARTESIAN_POINT('',(59.6095124682004,72.6054650011681,197.526481344607));
#26661=CARTESIAN_POINT('Origin',(59.7044966368782,72.3742118764312,197.526481344607));
#26662=CARTESIAN_POINT('',(59.4770762970785,72.2703851503661,183.174071706053));
#26663=CARTESIAN_POINT('Origin',(60.7314620557179,72.7960243673124,207.276481344607));
#26664=CARTESIAN_POINT('',(60.7314620557179,72.7960243673124,207.526481344607));
#26665=CARTESIAN_POINT('Origin',(60.7314620557179,72.7960243673124,207.276481344607));
#26666=CARTESIAN_POINT('Origin',(60.7314620557179,72.7960243673124,207.276481344607));
#26667=CARTESIAN_POINT('Origin',(79.4109822996944,61.2444364483471,207.276481344607));
#26668=CARTESIAN_POINT('',(79.1616957861817,61.2255622813273,207.276481344607));
#26669=CARTESIAN_POINT('Origin',(79.4109822996944,61.2444364483471,207.276481344607));
#26670=CARTESIAN_POINT('Origin',(79.4109822996944,61.2444364483471,207.276481344607));
#26671=CARTESIAN_POINT('Origin',(59.0227228960185,72.0941823110984,207.276481344607));
#26672=CARTESIAN_POINT('',(92.090597372954,85.676375289928,207.526481344607));
#26673=CARTESIAN_POINT('',(58.9277387273407,72.3254354358353,207.276481344607));
#26674=CARTESIAN_POINT('Origin',(77.215862801455,80.368869783441,207.276481344607));
#26675=CARTESIAN_POINT('',(77.8314138265035,62.2386587372839,207.526481344607));
#26676=CARTESIAN_POINT('Origin',(77.215862801455,80.368869783441,207.526481344607));
#26677=CARTESIAN_POINT('Origin',(77.8314138265035,62.2386587372839,207.276481344607));
#26678=CARTESIAN_POINT('Origin',(79.3126846293658,62.5427283061288,202.246481278135));
#26679=CARTESIAN_POINT('',(79.269084407634,62.9797812149621,197.285998194441));
#26680=CARTESIAN_POINT('',(79.269084625537,62.9797812385235,197.285998250943));
#26681=CARTESIAN_POINT('',(79.0497526609435,62.7041032964174,197.526481344555));
#26682=CARTESIAN_POINT('Ctrl Pts',(79.2690841890442,62.9797811913385,197.285998137443));
#26683=CARTESIAN_POINT('Ctrl Pts',(79.2680101135346,62.9796124948256,197.28708977948));
#26684=CARTESIAN_POINT('Ctrl Pts',(79.2677145897312,62.9795570615422,197.287528959389));
#26685=CARTESIAN_POINT('Ctrl Pts',(79.2647461981928,62.979070560001,197.290407185081));
#26686=CARTESIAN_POINT('Ctrl Pts',(79.2583629307362,62.9780074907501,197.296918746928));
#26687=CARTESIAN_POINT('Ctrl Pts',(79.2073485996536,62.965904807744,197.349058583512));
#26688=CARTESIAN_POINT('Ctrl Pts',(79.167673145419,62.9448626151971,197.390549949234));
#26689=CARTESIAN_POINT('Ctrl Pts',(79.1094927588433,62.8917379729484,197.452930411033));
#26690=CARTESIAN_POINT('Ctrl Pts',(79.0888676765804,62.8638759507458,197.475678618859));
#26691=CARTESIAN_POINT('Ctrl Pts',(79.0631009548931,62.8095576185035,197.505476436035));
#26692=CARTESIAN_POINT('Ctrl Pts',(79.05498120433,62.7835430926837,197.515495462576));
#26693=CARTESIAN_POINT('Ctrl Pts',(79.0490474931402,62.7385988418192,197.524688969095));
#26694=CARTESIAN_POINT('Ctrl Pts',(79.0485021933496,62.7213503394443,197.526481344716));
#26695=CARTESIAN_POINT('Ctrl Pts',(79.0497526616462,62.7041032964684,197.526481344607));
#26696=CARTESIAN_POINT('',(79.0498116915969,62.7033067469324,197.526481344607));
#26697=CARTESIAN_POINT('',(79.0498116915969,62.7033067469324,197.526481344607));
#26698=CARTESIAN_POINT('',(79.0778774854255,62.3326189234576,207.276481344607));
#26699=CARTESIAN_POINT('Origin',(79.4663159635354,60.513599631853,207.276481344607));
#26700=CARTESIAN_POINT('',(79.2170294500227,60.4947254648331,207.276481344607));
#26701=CARTESIAN_POINT('',(78.4136904864483,74.416482600992,207.526481344607));
#26702=CARTESIAN_POINT('Origin',(79.4109822996944,61.2444364483471,183.174071706053));
#26703=CARTESIAN_POINT('',(79.1624331548021,61.2175417913808,197.526481344607));
#26704=CARTESIAN_POINT('',(79.4394903451261,60.996067184255,197.276481344607));
#26705=CARTESIAN_POINT('Ctrl Pts',(79.1624331548021,61.2175417913808,197.526481344607));
#26706=CARTESIAN_POINT('Ctrl Pts',(79.162489527609,61.2170208175323,197.526481344607));
#26707=CARTESIAN_POINT('Ctrl Pts',(79.1625475669022,61.2164997575336,197.526479697129));
#26708=CARTESIAN_POINT('Ctrl Pts',(79.165273682838,61.1927066885413,197.526329043289));
#26709=CARTESIAN_POINT('Ctrl Pts',(79.1711458432171,61.1703503723531,197.522897090167));
#26710=CARTESIAN_POINT('Ctrl Pts',(79.1895930449751,61.125436422321,197.509425478113));
#26711=CARTESIAN_POINT('Ctrl Pts',(79.2026963979944,61.1041534241107,197.498728624379));
#26712=CARTESIAN_POINT('Ctrl Pts',(79.2378473596214,61.0613284405156,197.468545557741));
#26713=CARTESIAN_POINT('Ctrl Pts',(79.261292025071,61.0422175308465,197.447428878784));
#26714=CARTESIAN_POINT('Ctrl Pts',(79.3093010383479,61.014436050085,197.403006214921));
#26715=CARTESIAN_POINT('Ctrl Pts',(79.3340918218441,61.0052029860052,197.379534368409));
#26716=CARTESIAN_POINT('Ctrl Pts',(79.3849773214833,60.9943703469743,197.330483552621));
#26717=CARTESIAN_POINT('Ctrl Pts',(79.4114128508792,60.9930900494331,197.304533630738));
#26718=CARTESIAN_POINT('Ctrl Pts',(79.4379995190252,60.9958994640783,197.277971923767));
#26719=CARTESIAN_POINT('Ctrl Pts',(79.4387451263528,60.9959816473802,197.277226632397));
#26720=CARTESIAN_POINT('Ctrl Pts',(79.439490345126,60.996067184255,197.276481344607));
#26721=CARTESIAN_POINT('',(79.4394903451261,60.996067184255,183.174071706053));
#26722=CARTESIAN_POINT('',(79.1616957861817,61.2255622813273,197.526481344607));
#26723=CARTESIAN_POINT('',(79.1616957861817,61.2255622813273,197.526481344607));
#26724=CARTESIAN_POINT('Origin',(79.4109822996944,61.2444364483471,197.526481344607));
#26725=CARTESIAN_POINT('Origin',(77.215862801455,80.368869783441,207.276481344607));
#26726=CARTESIAN_POINT('Origin',(77.215862801455,80.368869783441,207.526481344607));
#26727=CARTESIAN_POINT('',(72.6073599718767,61.4212656692062,207.276481344607));
#26728=CARTESIAN_POINT('Origin',(77.215862801455,80.368869783441,207.276481344607));
#26729=CARTESIAN_POINT('Origin',(77.215862801455,80.368869783441,207.276481344607));
#26730=CARTESIAN_POINT('Origin',(77.8314138265035,62.2386587372839,207.276481344607));
#26731=CARTESIAN_POINT('',(78.0807003400161,62.2575329043037,207.276481344607));
#26732=CARTESIAN_POINT('Origin',(77.8314138265035,62.2386587372839,207.276481344607));
#26733=CARTESIAN_POINT('Origin',(77.8314138265035,62.2386587372839,207.276481344607));
#26734=CARTESIAN_POINT('Origin',(77.215862801455,80.368869783441,197.276481344607));
#26735=CARTESIAN_POINT('',(77.7943741989354,62.8685427940256,197.285998169697));
#26736=CARTESIAN_POINT('',(78.052583306941,62.6288859648788,197.526481344578));
#26737=CARTESIAN_POINT('Ctrl Pts',(77.7943744744014,62.8685428093252,197.285998007207));
#26738=CARTESIAN_POINT('Ctrl Pts',(77.7953871004452,62.868537531901,197.287014717876));
#26739=CARTESIAN_POINT('Ctrl Pts',(77.7954406625158,62.868511022385,197.287634888787));
#26740=CARTESIAN_POINT('Ctrl Pts',(77.796910574736,62.8685035682567,197.288828524609));
#26741=CARTESIAN_POINT('Ctrl Pts',(77.7979976652988,62.8684929763872,197.289840350133));
#26742=CARTESIAN_POINT('Ctrl Pts',(77.8029322243904,62.8683662151868,197.294649285739));
#26743=CARTESIAN_POINT('Ctrl Pts',(77.8299951625382,62.868403557902,197.321793962165));
#26744=CARTESIAN_POINT('Ctrl Pts',(77.9036914339881,62.8468136488644,197.394186937533));
#26745=CARTESIAN_POINT('Ctrl Pts',(77.9394990504386,62.8264863037409,197.428597657109));
#26746=CARTESIAN_POINT('Ctrl Pts',(77.9924180066599,62.7775563807812,197.477895540356));
#26747=CARTESIAN_POINT('Ctrl Pts',(78.0113061411039,62.7525744408473,197.494874374673));
#26748=CARTESIAN_POINT('Ctrl Pts',(78.0365242286412,62.7030752536208,197.516246243239));
#26749=CARTESIAN_POINT('Ctrl Pts',(78.0449179730812,62.6789343473944,197.522744141435));
#26750=CARTESIAN_POINT('Ctrl Pts',(78.0509156442943,62.6450929646504,197.526084814193));
#26751=CARTESIAN_POINT('Ctrl Pts',(78.0519478312877,62.6369945577109,197.526481344688));
#26752=CARTESIAN_POINT('Ctrl Pts',(78.052583303161,62.6288859645826,197.526481344607));
#26753=CARTESIAN_POINT('Origin',(77.215862801455,80.368869783441,197.526481344607));
#26754=CARTESIAN_POINT('Origin',(77.215862801455,80.368869783441,197.285998250943));
#26755=CARTESIAN_POINT('Origin',(77.215862801455,80.368869783441,197.276481344607));
#26756=CARTESIAN_POINT('',(78.1650046288044,61.1422832483439,197.526481344607));
#26757=CARTESIAN_POINT('',(77.9243166636283,60.8817434400015,197.276481344607));
#26758=CARTESIAN_POINT('Ctrl Pts',(78.1650046288044,61.1422832483439,197.526481344607));
#26759=CARTESIAN_POINT('Ctrl Pts',(78.16502706682,61.1417597140309,197.526481344607));
#26760=CARTESIAN_POINT('Ctrl Pts',(78.1650478701437,61.1412358444854,197.526479697129));
#26761=CARTESIAN_POINT('Ctrl Pts',(78.1659227895184,61.1173030979625,197.52632904329));
#26762=CARTESIAN_POINT('Ctrl Pts',(78.1634716970727,61.0943187709797,197.522897090169));
#26763=CARTESIAN_POINT('Ctrl Pts',(78.1519727272435,61.047145305419,197.509425478116));
#26764=CARTESIAN_POINT('Ctrl Pts',(78.142211259418,61.0241370977738,197.498728624383));
#26765=CARTESIAN_POINT('Ctrl Pts',(78.1138841938284,60.9765225340547,197.468545557748));
#26766=CARTESIAN_POINT('Ctrl Pts',(78.0935725712605,60.9541101001165,197.447428878792));
#26767=CARTESIAN_POINT('Ctrl Pts',(78.0502757384727,60.9194393588524,197.403006214929));
#26768=CARTESIAN_POINT('Ctrl Pts',(78.0271510587944,60.9065909500587,197.379534368416));
#26769=CARTESIAN_POINT('Ctrl Pts',(77.9784671177831,60.8882455410985,197.330483552625));
#26770=CARTESIAN_POINT('Ctrl Pts',(77.9525229939557,60.8830130642432,197.304533630717));
#26771=CARTESIAN_POINT('Ctrl Pts',(77.9258157775659,60.8818013184771,197.277971923771));
#26772=CARTESIAN_POINT('Ctrl Pts',(77.9250662801213,60.8817706922854,197.277226632395));
#26773=CARTESIAN_POINT('Ctrl Pts',(77.9243166636283,60.8817434400015,197.276481344607));
#26774=CARTESIAN_POINT('Origin',(77.215862801455,80.368869783441,197.276481344607));
#26775=CARTESIAN_POINT('Origin',(77.215862801455,80.368869783441,197.526481344607));
#26776=CARTESIAN_POINT('Origin',(77.9774013323172,60.3104827122258,207.276481344607));
#26777=CARTESIAN_POINT('',(78.2266878458299,60.3293568792457,207.276481344607));
#26778=CARTESIAN_POINT('',(76.9179714053723,74.3032375988726,207.526481344607));
#26779=CARTESIAN_POINT('Origin',(77.8169349762247,62.4298984090937,202.246481276341));
#26780=CARTESIAN_POINT('',(77.8070980354658,62.6991535160838,201.74111193235));
#26781=CARTESIAN_POINT('',(78.0526338951397,62.6282293266983,197.526481344607));
#26782=CARTESIAN_POINT('',(78.0526338951397,62.6282293266983,197.526481344607));
#26783=CARTESIAN_POINT('',(78.0525833124769,62.6288859405896,197.52648134452));
#26784=CARTESIAN_POINT('Origin',(77.9152339218055,61.1315783931226,183.174071706053));
#26785=CARTESIAN_POINT('',(78.1645204353182,61.1504525601425,197.526481344607));
#26786=CARTESIAN_POINT('Origin',(77.9152339218055,61.1315783931226,197.526481344607));
#26787=CARTESIAN_POINT('',(78.1645204353182,61.1504525601425,197.526481344607));
#26788=CARTESIAN_POINT('',(77.9243166636283,60.8817434400015,183.174071706053));
#26789=CARTESIAN_POINT('Origin',(77.215862801455,80.368869783441,194.876481344607));
#26790=CARTESIAN_POINT('',(69.7713582305978,49.7612015989078,194.876481344607));
#26791=CARTESIAN_POINT('Origin',(77.215862801455,80.368869783441,194.876481344607));
#26792=CARTESIAN_POINT('',(69.8304416002078,50.0041196003723,195.126481344607));
#26793=CARTESIAN_POINT('Origin',(69.8304416002078,50.0041196003723,194.876481344607));
#26794=CARTESIAN_POINT('Origin',(77.215862801455,80.368869783441,195.126481344607));
#26795=CARTESIAN_POINT('Origin',(77.215862801455,80.368869783441,197.526481344607));
#26796=CARTESIAN_POINT('',(96.4310252714059,76.2098674030624,197.526481344607));
#26797=CARTESIAN_POINT('',(96.194691792966,75.2381953972042,197.526481344607));
#26798=CARTESIAN_POINT('Origin',(96.194691792966,75.2381953972042,197.526481344607));
#26799=CARTESIAN_POINT('Origin',(96.4310252714059,76.2098674030624,197.526481344607));
#26800=CARTESIAN_POINT('Origin',(78.4583471591332,61.9901304421851,197.526481344607));
#26801=CARTESIAN_POINT('',(79.2170294500227,60.4947254648331,197.526481344607));
#26802=CARTESIAN_POINT('',(78.2266878458299,60.3293568792457,197.526481344607));
#26803=CARTESIAN_POINT('Origin',(79.2170294500227,60.4947254648331,197.526481344607));
#26804=CARTESIAN_POINT('Origin',(78.2266878458299,60.3293568792457,197.526481344607));
#26805=CARTESIAN_POINT('Origin',(60.1155076543353,73.5090907238581,197.526481344607));
#26806=CARTESIAN_POINT('',(58.9277387273407,72.3254354358353,197.526481344607));
#26807=CARTESIAN_POINT('',(58.4644314704952,73.2162045685788,197.526481344607));
#26808=CARTESIAN_POINT('Origin',(58.9277387273407,72.3254354358353,197.526481344607));
#26809=CARTESIAN_POINT('Origin',(58.4644314704952,73.2162045685788,197.526481344607));
#26810=CARTESIAN_POINT('Origin',(65.4024407590908,94.5137222468193,197.526481344607));
#26811=CARTESIAN_POINT('',(63.9096769005376,95.2775880252097,197.526481344607));
#26812=CARTESIAN_POINT('',(64.6136788727654,95.9934822109618,197.526481344607));
#26813=CARTESIAN_POINT('Origin',(63.9096769005376,95.2775880252097,197.526481344607));
#26814=CARTESIAN_POINT('Origin',(64.6136788727654,95.9934822109618,197.526481344607));
#26815=CARTESIAN_POINT('Origin',(87.0127846188746,95.9763381675038,197.526481344607));
#26816=CARTESIAN_POINT('',(87.277974744106,97.6320884694148,197.526481344607));
#26817=CARTESIAN_POINT('',(88.1763791479352,97.1837662758145,197.526481344607));
#26818=CARTESIAN_POINT('Origin',(87.277974744106,97.6320884694148,197.526481344607));
#26819=CARTESIAN_POINT('Origin',(88.1763791479352,97.1837662758145,197.526481344607));
#26820=CARTESIAN_POINT('Origin',(94.9974604855648,76.0439671336079,193.776481344607));
#26821=CARTESIAN_POINT('',(72.8909601516219,62.5872720993312,193.776481344607));
#26822=CARTESIAN_POINT('Origin',(77.215862801455,80.368869783441,193.776481344607));
#26823=CARTESIAN_POINT('Origin',(77.215862801455,80.368869783441,194.576481344607));
#26824=CARTESIAN_POINT('',(73.0800269287566,63.3646096809225,194.576145266601));
#26825=CARTESIAN_POINT('Origin',(77.215862801455,80.368869783441,194.576145266601));
#26826=CARTESIAN_POINT('Origin',(72.890960162688,62.587272144829,194.576481344607));
#26827=CARTESIAN_POINT('Origin',(77.215862801455,80.368869783441,183.174071706053));
#26828=CARTESIAN_POINT('',(73.0800269287565,63.3646096809226,183.174071706053));
#26829=CARTESIAN_POINT('Origin',(77.215862801455,80.368869783441,197.026481344607));
#26830=CARTESIAN_POINT('',(81.3516986741534,97.3731298859594,197.026481344607));
#26831=CARTESIAN_POINT('Origin',(96.1634669156899,75.7603669538627,207.526481344607));
#26832=CARTESIAN_POINT('Origin',(77.215862801455,80.368869783441,183.174071706053));
#26833=CARTESIAN_POINT('',(72.6073599718767,61.4212656692062,183.174071706053));
#26834=CARTESIAN_POINT('Origin',(107.823530985988,72.9243652125838,195.126481344607));
#26835=CARTESIAN_POINT('Origin',(77.215862801455,80.368869783441,183.174071706053));
#26836=CARTESIAN_POINT('',(69.7713582305978,49.7612015989078,183.174071706053));
#26837=CARTESIAN_POINT('Origin',(96.1634669156899,75.7603669538627,207.526481344607));
#26838=CARTESIAN_POINT('Origin',(96.1634669156899,75.7603669538627,207.526481344607));
#26839=CARTESIAN_POINT('Origin',(96.1634669156899,75.7603669538627,207.526481344607));
#26840=CARTESIAN_POINT('Origin',(96.1634669156899,75.7603669538627,207.526481344607));
#26841=CARTESIAN_POINT('',(0.,0.,0.));
#26842=CARTESIAN_POINT('Origin',(17.738300751771,49.437062129158,214.5));
#26843=CARTESIAN_POINT('',(13.738300751771,49.437062129158,214.5));
#26844=CARTESIAN_POINT('',(17.738300751771,53.437062129158,214.5));
#26845=CARTESIAN_POINT('Origin',(17.738300751771,49.437062129158,214.5));
#26846=CARTESIAN_POINT('',(13.738300751771,49.437062129158,212.5));
#26847=CARTESIAN_POINT('',(13.738300751771,49.437062129158,214.5));
#26848=CARTESIAN_POINT('',(17.738300751771,53.437062129158,212.5));
#26849=CARTESIAN_POINT('Origin',(17.738300751771,49.437062129158,212.5));
#26850=CARTESIAN_POINT('',(17.738300751771,53.437062129158,212.5));
#26851=CARTESIAN_POINT('Origin',(17.738300751771,35.437062129158,214.5));
#26852=CARTESIAN_POINT('',(17.738300751771,31.437062129158,214.5));
#26853=CARTESIAN_POINT('',(13.738300751771,35.437062129158,214.5));
#26854=CARTESIAN_POINT('Origin',(17.738300751771,35.437062129158,214.5));
#26855=CARTESIAN_POINT('',(17.738300751771,31.437062129158,212.5));
#26856=CARTESIAN_POINT('',(17.738300751771,31.437062129158,214.5));
#26857=CARTESIAN_POINT('',(13.738300751771,35.437062129158,212.5));
#26858=CARTESIAN_POINT('Origin',(17.738300751771,35.437062129158,212.5));
#26859=CARTESIAN_POINT('',(13.738300751771,35.437062129158,212.5));
#26860=CARTESIAN_POINT('Origin',(41.738300751771,35.437062129158,214.5));
#26861=CARTESIAN_POINT('',(45.738300751771,35.437062129158,214.5));
#26862=CARTESIAN_POINT('',(41.738300751771,31.437062129158,214.5));
#26863=CARTESIAN_POINT('Origin',(41.738300751771,35.437062129158,214.5));
#26864=CARTESIAN_POINT('',(45.738300751771,35.437062129158,212.5));
#26865=CARTESIAN_POINT('',(45.738300751771,35.437062129158,214.5));
#26866=CARTESIAN_POINT('',(41.738300751771,31.437062129158,212.5));
#26867=CARTESIAN_POINT('Origin',(41.738300751771,35.437062129158,212.5));
#26868=CARTESIAN_POINT('',(41.738300751771,31.437062129158,212.5));
#26869=CARTESIAN_POINT('Origin',(41.738300751771,49.437062129158,214.5));
#26870=CARTESIAN_POINT('',(41.738300751771,53.437062129158,214.5));
#26871=CARTESIAN_POINT('',(45.738300751771,49.437062129158,214.5));
#26872=CARTESIAN_POINT('Origin',(41.738300751771,49.437062129158,214.5));
#26873=CARTESIAN_POINT('',(41.738300751771,53.437062129158,212.5));
#26874=CARTESIAN_POINT('',(41.738300751771,53.437062129158,214.5));
#26875=CARTESIAN_POINT('',(45.738300751771,49.437062129158,212.5));
#26876=CARTESIAN_POINT('Origin',(41.738300751771,49.437062129158,212.5));
#26877=CARTESIAN_POINT('',(45.738300751771,49.437062129158,212.5));
#26878=CARTESIAN_POINT('Origin',(1.3592091877994,36.437062129158,214.5));
#26879=CARTESIAN_POINT('',(5.23464599548021,35.4466129635399,214.5));
#26880=CARTESIAN_POINT('',(1.3592091877994,32.437062129158,214.5));
#26881=CARTESIAN_POINT('Origin',(1.3592091877994,36.437062129158,214.5));
#26882=CARTESIAN_POINT('',(5.23464599548021,35.4466129635399,212.5));
#26883=CARTESIAN_POINT('',(5.23464599548021,35.4466129635399,214.5));
#26884=CARTESIAN_POINT('',(1.3592091877994,32.437062129158,212.5));
#26885=CARTESIAN_POINT('Origin',(1.3592091877994,36.437062129158,212.5));
#26886=CARTESIAN_POINT('',(1.3592091877994,32.437062129158,212.5));
#26887=CARTESIAN_POINT('Origin',(42.977211794544,76.437062129158,214.5));
#26888=CARTESIAN_POINT('',(45.625792720535,73.4395599892964,214.5));
#26889=CARTESIAN_POINT('',(42.977211794544,72.437062129158,214.5));
#26890=CARTESIAN_POINT('Origin',(42.977211794544,76.437062129158,214.5));
#26891=CARTESIAN_POINT('',(45.625792720535,73.4395599892964,212.5));
#26892=CARTESIAN_POINT('',(45.625792720535,73.4395599892964,214.5));
#26893=CARTESIAN_POINT('',(42.977211794544,72.437062129158,212.5));
#26894=CARTESIAN_POINT('Origin',(42.977211794544,76.437062129158,212.5));
#26895=CARTESIAN_POINT('',(42.977211794544,72.437062129158,212.5));
#26896=CARTESIAN_POINT('Origin',(-112.45844945829,-38.2430904326252,213.4));
#26897=CARTESIAN_POINT('',(-110.85844945829,-38.2430904326252,213.4));
#26898=CARTESIAN_POINT('',(-114.05844945829,-38.2430904326252,213.4));
#26899=CARTESIAN_POINT('Origin',(-112.45844945829,-38.2430904326252,213.4));
#26900=CARTESIAN_POINT('Origin',(-112.45844945829,-38.2430904326252,213.4));
#26901=CARTESIAN_POINT('',(-115.15844945829,-38.2430904326252,214.5));
#26902=CARTESIAN_POINT('',(-114.05844945829,-38.2430904326252,213.4));
#26903=CARTESIAN_POINT('Origin',(-112.45844945829,-38.2430904326252,214.5));
#26904=CARTESIAN_POINT('Origin',(-110.126903127,25.6553383360753,213.4));
#26905=CARTESIAN_POINT('',(-108.526903127,25.6553383360753,213.4));
#26906=CARTESIAN_POINT('',(-111.726903127,25.6553383360753,213.4));
#26907=CARTESIAN_POINT('Origin',(-110.126903127,25.6553383360753,213.4));
#26908=CARTESIAN_POINT('Origin',(-110.126903127,25.6553383360753,213.4));
#26909=CARTESIAN_POINT('',(-112.826903127,25.6553383360753,214.5));
#26910=CARTESIAN_POINT('',(-111.726903127,25.6553383360753,213.4));
#26911=CARTESIAN_POINT('Origin',(-110.126903127,25.6553383360753,214.5));
#26912=CARTESIAN_POINT('Origin',(-37.5407744425955,-7.8397685706167,213.4));
#26913=CARTESIAN_POINT('',(-35.9407744425954,-7.8397685706167,213.4));
#26914=CARTESIAN_POINT('',(-39.1407744425955,-7.8397685706167,213.4));
#26915=CARTESIAN_POINT('Origin',(-37.5407744425955,-7.8397685706167,213.4));
#26916=CARTESIAN_POINT('Origin',(-37.5407744425955,-7.8397685706167,213.4));
#26917=CARTESIAN_POINT('',(-40.2407744425955,-7.8397685706167,214.5));
#26918=CARTESIAN_POINT('',(-39.1407744425955,-7.8397685706167,213.4));
#26919=CARTESIAN_POINT('Origin',(-37.5407744425955,-7.8397685706167,214.5));
#26920=CARTESIAN_POINT('Origin',(40.4592255574045,-7.8397685706167,213.4));
#26921=CARTESIAN_POINT('',(42.0592255574045,-7.8397685706167,213.4));
#26922=CARTESIAN_POINT('',(38.8592255574045,-7.8397685706167,213.4));
#26923=CARTESIAN_POINT('Origin',(40.4592255574045,-7.8397685706167,213.4));
#26924=CARTESIAN_POINT('Origin',(40.4592255574045,-7.8397685706167,213.4));
#26925=CARTESIAN_POINT('',(37.7592255574045,-7.8397685706167,214.5));
#26926=CARTESIAN_POINT('',(38.8592255574045,-7.8397685706167,213.4));
#26927=CARTESIAN_POINT('Origin',(40.4592255574045,-7.8397685706167,214.5));
#26928=CARTESIAN_POINT('Origin',(73.324673000048,-35.1598100783688,213.4));
#26929=CARTESIAN_POINT('',(74.924673000048,-35.1598100783688,213.4));
#26930=CARTESIAN_POINT('',(71.724673000048,-35.1598100783688,213.4));
#26931=CARTESIAN_POINT('Origin',(73.324673000048,-35.1598100783688,213.4));
#26932=CARTESIAN_POINT('Origin',(73.324673000048,-35.1598100783688,213.4));
#26933=CARTESIAN_POINT('',(70.624673000048,-35.1598100783688,214.5));
#26934=CARTESIAN_POINT('',(71.724673000048,-35.1598100783688,213.4));
#26935=CARTESIAN_POINT('Origin',(73.324673000048,-35.1598100783688,214.5));
#26936=CARTESIAN_POINT('Origin',(54.6355073401705,34.895083038275,213.4));
#26937=CARTESIAN_POINT('',(56.2355073401705,34.895083038275,213.4));
#26938=CARTESIAN_POINT('',(53.0355073401705,34.895083038275,213.4));
#26939=CARTESIAN_POINT('Origin',(54.6355073401705,34.895083038275,213.4));
#26940=CARTESIAN_POINT('Origin',(54.6355073401705,34.895083038275,213.4));
#26941=CARTESIAN_POINT('',(51.9355073401705,34.895083038275,214.5));
#26942=CARTESIAN_POINT('',(53.0355073401705,34.895083038275,213.4));
#26943=CARTESIAN_POINT('Origin',(54.6355073401705,34.895083038275,214.5));
#26944=CARTESIAN_POINT('Origin',(5.7207051493956,10.2688129333875,213.4));
#26945=CARTESIAN_POINT('',(7.32070514939562,10.2688129333875,213.4));
#26946=CARTESIAN_POINT('',(4.1207051493956,10.2688129333875,213.4));
#26947=CARTESIAN_POINT('Origin',(5.7207051493956,10.2688129333875,213.4));
#26948=CARTESIAN_POINT('Origin',(5.7207051493956,10.2688129333875,213.4));
#26949=CARTESIAN_POINT('',(3.02070514939559,10.2688129333875,214.5));
#26950=CARTESIAN_POINT('',(4.1207051493956,10.2688129333875,213.4));
#26951=CARTESIAN_POINT('Origin',(5.7207051493956,10.2688129333875,214.5));
#26952=CARTESIAN_POINT('Origin',(77.738300751771,81.5680647192538,213.4));
#26953=CARTESIAN_POINT('',(79.338300751771,81.5680647192538,213.4));
#26954=CARTESIAN_POINT('',(76.138300751771,81.5680647192538,213.4));
#26955=CARTESIAN_POINT('Origin',(77.738300751771,81.5680647192538,213.4));
#26956=CARTESIAN_POINT('Origin',(77.738300751771,81.5680647192538,213.4));
#26957=CARTESIAN_POINT('',(75.038300751771,81.5680647192538,214.5));
#26958=CARTESIAN_POINT('',(76.138300751771,81.5680647192538,213.4));
#26959=CARTESIAN_POINT('Origin',(77.738300751771,81.5680647192538,214.5));
#26960=CARTESIAN_POINT('Origin',(39.747079812151,62.1619809501,213.4));
#26961=CARTESIAN_POINT('',(41.347079812151,62.1619809501,213.4));
#26962=CARTESIAN_POINT('',(38.147079812151,62.1619809501,213.4));
#26963=CARTESIAN_POINT('Origin',(39.747079812151,62.1619809501,213.4));
#26964=CARTESIAN_POINT('Origin',(39.747079812151,62.1619809501,213.4));
#26965=CARTESIAN_POINT('',(37.047079812151,62.1619809501,214.5));
#26966=CARTESIAN_POINT('',(38.147079812151,62.1619809501,213.4));
#26967=CARTESIAN_POINT('Origin',(39.747079812151,62.1619809501,214.5));
#26968=CARTESIAN_POINT('Origin',(25.1879034811638,63.7619809501,213.4));
#26969=CARTESIAN_POINT('',(27.287903481164,63.7619809501,213.4));
#26970=CARTESIAN_POINT('',(23.0879034811638,63.7619809501,213.4));
#26971=CARTESIAN_POINT('Origin',(25.1879034811638,63.7619809501,213.4));
#26972=CARTESIAN_POINT('Origin',(25.1879034811638,63.7619809501,213.4));
#26973=CARTESIAN_POINT('',(21.9879034811638,63.7619809501,214.5));
#26974=CARTESIAN_POINT('',(23.0879034811638,63.7619809501,213.4));
#26975=CARTESIAN_POINT('Origin',(25.1879034811638,63.7619809501,214.5));
#26976=CARTESIAN_POINT('Origin',(-55.2792948506043,10.2688129333875,213.4));
#26977=CARTESIAN_POINT('',(-53.6792948506043,10.2688129333875,213.4));
#26978=CARTESIAN_POINT('',(-56.8792948506043,10.2688129333875,213.4));
#26979=CARTESIAN_POINT('Origin',(-55.2792948506043,10.2688129333875,213.4));
#26980=CARTESIAN_POINT('Origin',(-55.2792948506043,10.2688129333875,213.4));
#26981=CARTESIAN_POINT('',(-57.9792948506043,10.2688129333875,214.5));
#26982=CARTESIAN_POINT('',(-56.8792948506043,10.2688129333875,213.4));
#26983=CARTESIAN_POINT('Origin',(-55.2792948506043,10.2688129333875,214.5));
#26984=CARTESIAN_POINT('Origin',(-11.261699248229,29.437062129158,213.4));
#26985=CARTESIAN_POINT('',(-9.66169924822899,29.437062129158,213.4));
#26986=CARTESIAN_POINT('',(-12.861699248229,29.437062129158,213.4));
#26987=CARTESIAN_POINT('Origin',(-11.261699248229,29.437062129158,213.4));
#26988=CARTESIAN_POINT('Origin',(-11.261699248229,29.437062129158,213.4));
#26989=CARTESIAN_POINT('',(-13.961699248229,29.437062129158,214.5));
#26990=CARTESIAN_POINT('',(-12.861699248229,29.437062129158,213.4));
#26991=CARTESIAN_POINT('Origin',(-11.261699248229,29.437062129158,214.5));
#26992=CARTESIAN_POINT('Origin',(-65.261699248229,29.437062129158,213.4));
#26993=CARTESIAN_POINT('',(-63.661699248229,29.437062129158,213.4));
#26994=CARTESIAN_POINT('',(-66.861699248229,29.437062129158,213.4));
#26995=CARTESIAN_POINT('Origin',(-65.261699248229,29.437062129158,213.4));
#26996=CARTESIAN_POINT('Origin',(-65.261699248229,29.437062129158,213.4));
#26997=CARTESIAN_POINT('',(-67.961699248229,29.437062129158,214.5));
#26998=CARTESIAN_POINT('',(-66.861699248229,29.437062129158,213.4));
#26999=CARTESIAN_POINT('Origin',(-65.261699248229,29.437062129158,214.5));
#27000=CARTESIAN_POINT('Origin',(-123.261699248229,-48.562937870842,210.5));
#27001=CARTESIAN_POINT('',(57.335333187315,-46.562937870842,210.5));
#27002=CARTESIAN_POINT('',(57.335333187315,-48.562937870842,210.5));
#27003=CARTESIAN_POINT('',(57.335333187315,-48.562937870842,210.5));
#27004=CARTESIAN_POINT('',(67.799693512506,-48.562937870842,210.5));
#27005=CARTESIAN_POINT('',(57.335333187315,-48.562937870842,210.5));
#27006=CARTESIAN_POINT('',(67.799693512506,-46.562937870842,210.5));
#27007=CARTESIAN_POINT('',(67.799693512506,-48.562937870842,210.5));
#27008=CARTESIAN_POINT('',(57.335333187315,-46.562937870842,210.5));
#27009=CARTESIAN_POINT('Origin',(-88.261699248229,-31.562937870842,251.410152916687));
#27010=CARTESIAN_POINT('',(-88.261699248229,-47.762937870842,194.5));
#27011=CARTESIAN_POINT('',(-88.261699248229,-48.562937870842,195.3));
#27012=CARTESIAN_POINT('Origin',(-88.261699248229,-47.762937870842,195.3));
#27013=CARTESIAN_POINT('',(-88.261699248229,-48.562937870842,212.5));
#27014=CARTESIAN_POINT('',(-88.261699248229,-48.562937870842,251.410152916687));
#27015=CARTESIAN_POINT('',(-88.261699248229,-45.7629378708421,212.5));
#27016=CARTESIAN_POINT('',(-88.261699248229,-31.562937870842,212.5));
#27017=CARTESIAN_POINT('',(-88.261699248229,-46.5629378708421,211.7));
#27018=CARTESIAN_POINT('Origin',(-88.261699248229,-45.7629378708421,211.7));
#27019=CARTESIAN_POINT('',(-88.261699248229,-46.562937870842,197.3));
#27020=CARTESIAN_POINT('',(-88.261699248229,-46.562937870842,214.5));
#27021=CARTESIAN_POINT('',(-88.261699248229,-45.762937870842,196.5));
#27022=CARTESIAN_POINT('Origin',(-88.261699248229,-45.762937870842,197.3));
#27023=CARTESIAN_POINT('',(-88.261699248229,-31.562937870842,196.5));
#27024=CARTESIAN_POINT('',(-88.261699248229,-46.5629378708419,196.5));
#27025=CARTESIAN_POINT('',(-88.261699248229,-31.562937870842,194.5));
#27026=CARTESIAN_POINT('',(-88.261699248229,-31.562937870842,251.410152916687));
#27027=CARTESIAN_POINT('',(-88.261699248229,-31.562937870842,194.5));
#27028=CARTESIAN_POINT('Origin',(-123.261699248229,-48.562937870842,196.5));
#27029=CARTESIAN_POINT('',(-33.261699248229,-45.762937870842,196.5));
#27030=CARTESIAN_POINT('',(-23.261699248229,-45.762937870842,196.5));
#27031=CARTESIAN_POINT('',(76.738300751771,-45.762937870842,196.5));
#27032=CARTESIAN_POINT('',(-23.261699248229,-47.762937870842,196.5));
#27033=CARTESIAN_POINT('',(-23.261699248229,-47.762937870842,196.5));
#27034=CARTESIAN_POINT('',(-33.261699248229,-47.762937870842,196.5));
#27035=CARTESIAN_POINT('',(-33.261699248229,-47.762937870842,196.5));
#27036=CARTESIAN_POINT('',(-33.261699248229,-31.562937870842,196.5));
#27037=CARTESIAN_POINT('Origin',(-23.261699248229,-47.762937870842,196.5));
#27038=CARTESIAN_POINT('',(-23.261699248229,-31.562937870842,194.5));
#27039=CARTESIAN_POINT('',(-23.261699248229,-47.762937870842,194.5));
#27040=CARTESIAN_POINT('',(-23.261699248229,-47.762937870842,194.5));
#27041=CARTESIAN_POINT('',(-23.261699248229,-47.762937870842,196.5));
#27042=CARTESIAN_POINT('',(-23.261699248229,-31.562937870842,196.5));
#27043=CARTESIAN_POINT('',(-23.261699248229,-47.762937870842,196.5));
#27044=CARTESIAN_POINT('',(-23.261699248229,-31.562937870842,196.5));
#27045=CARTESIAN_POINT('Origin',(-33.261699248229,-47.762937870842,196.5));
#27046=CARTESIAN_POINT('',(-33.261699248229,-47.762937870842,194.5));
#27047=CARTESIAN_POINT('',(-33.261699248229,-47.762937870842,194.5));
#27048=CARTESIAN_POINT('',(-33.261699248229,-47.762937870842,196.5));
#27049=CARTESIAN_POINT('Origin',(-33.261699248229,-31.562937870842,196.5));
#27050=CARTESIAN_POINT('',(-33.261699248229,-31.562937870842,194.5));
#27051=CARTESIAN_POINT('',(-33.261699248229,-31.562937870842,194.5));
#27052=CARTESIAN_POINT('',(-33.261699248229,-31.562937870842,196.5));
#27053=CARTESIAN_POINT('',(-33.261699248229,-31.562937870842,196.5));
#27054=CARTESIAN_POINT('',(-33.261699248229,-31.562937870842,196.5));
#27055=CARTESIAN_POINT('Origin',(82.241473619047,-45.762937870842,211.7));
#27056=CARTESIAN_POINT('',(53.335333187315,-46.562937870842,211.7));
#27057=CARTESIAN_POINT('',(53.335333187315,-46.562937870842,211.7));
#27058=CARTESIAN_POINT('',(53.335333187315,-45.762937870842,212.5));
#27059=CARTESIAN_POINT('',(-123.261699248229,-45.7629378708421,212.5));
#27060=CARTESIAN_POINT('Origin',(53.335333187315,-45.762937870842,211.7));
#27061=CARTESIAN_POINT('Origin',(70.6019681378195,-45.762937870842,197.3));
#27062=CARTESIAN_POINT('',(76.738300751771,-45.762937870842,196.5));
#27063=CARTESIAN_POINT('',(76.738300751771,-46.562937870842,197.3));
#27064=CARTESIAN_POINT('',(70.6019681378195,-46.562937870842,197.3));
#27065=CARTESIAN_POINT('',(76.738300751771,-45.762937870842,196.5));
#27066=CARTESIAN_POINT('Origin',(76.738300751771,-45.762937870842,197.3));
#27067=CARTESIAN_POINT('',(76.738300751771,-45.762937870842,196.5));
#27068=CARTESIAN_POINT('Origin',(82.241473619047,-47.762937870842,213.7));
#27069=CARTESIAN_POINT('',(-123.261699248229,-48.562937870842,213.7));
#27070=CARTESIAN_POINT('',(-123.261699248229,-47.762937870842,214.5));
#27071=CARTESIAN_POINT('Origin',(-123.261699248229,-47.762937870842,213.7));
#27072=CARTESIAN_POINT('',(57.335333187315,-48.562937870842,213.7));
#27073=CARTESIAN_POINT('',(-123.261699248229,-48.562937870842,213.7));
#27074=CARTESIAN_POINT('',(57.335333187315,-47.762937870842,214.5));
#27075=CARTESIAN_POINT('Origin',(57.335333187315,-47.762937870842,213.7));
#27076=CARTESIAN_POINT('',(57.335333187315,-47.762937870842,214.5));
#27077=CARTESIAN_POINT('Origin',(76.738300751771,-47.762937870842,195.3));
#27078=CARTESIAN_POINT('',(-123.261699248229,-47.762937870842,194.5));
#27079=CARTESIAN_POINT('',(76.738300751771,-47.762937870842,194.5));
#27080=CARTESIAN_POINT('',(-123.261699248229,-47.762937870842,194.5));
#27081=CARTESIAN_POINT('',(76.738300751771,-48.562937870842,195.3));
#27082=CARTESIAN_POINT('Origin',(76.738300751771,-47.762937870842,195.3));
#27083=CARTESIAN_POINT('',(76.738300751771,-48.562937870842,195.3));
#27084=CARTESIAN_POINT('Origin',(76.738300751771,-48.562937870842,212.5));
#27085=CARTESIAN_POINT('',(76.738300751771,-48.562937870842,212.5));
#27086=CARTESIAN_POINT('',(76.738300751771,-48.562937870842,212.5));
#27087=CARTESIAN_POINT('',(76.738300751771,-31.562937870842,194.5));
#27088=CARTESIAN_POINT('',(76.738300751771,-31.562937870842,194.5));
#27089=CARTESIAN_POINT('',(76.738300751771,-31.562937870842,196.5));
#27090=CARTESIAN_POINT('',(76.738300751771,-31.562937870842,196.5));
#27091=CARTESIAN_POINT('',(76.738300751771,-46.562937870842,196.5));
#27092=CARTESIAN_POINT('',(76.738300751771,-46.562937870842,212.5));
#27093=CARTESIAN_POINT('',(76.738300751771,-46.562937870842,212.5));
#27094=CARTESIAN_POINT('',(76.738300751771,-46.562937870842,212.5));
#27095=CARTESIAN_POINT('Origin',(76.738300751771,-46.562937870842,196.5));
#27096=CARTESIAN_POINT('',(76.738300751771,-31.562937870842,196.5));
#27097=CARTESIAN_POINT('Origin',(76.738300751771,-31.562937870842,196.5));
#27098=CARTESIAN_POINT('',(76.738300751771,-31.562937870842,194.5));
#27099=CARTESIAN_POINT('Origin',(76.738300751771,-31.562937870842,194.5));
#27100=CARTESIAN_POINT('Origin',(13.738300751771,53.437062129158,214.5));
#27101=CARTESIAN_POINT('',(13.738300751771,53.437062129158,212.5));
#27102=CARTESIAN_POINT('',(13.738300751771,53.437062129158,214.5));
#27103=CARTESIAN_POINT('Origin',(45.738300751771,53.437062129158,214.5));
#27104=CARTESIAN_POINT('',(45.738300751771,53.437062129158,214.5));
#27105=CARTESIAN_POINT('',(45.738300751771,53.437062129158,212.5));
#27106=CARTESIAN_POINT('Origin',(13.738300751771,31.437062129158,214.5));
#27107=CARTESIAN_POINT('',(13.738300751771,31.437062129158,214.5));
#27108=CARTESIAN_POINT('',(13.738300751771,31.437062129158,212.5));
#27109=CARTESIAN_POINT('Origin',(13.738300751771,53.437062129158,214.5));
#27110=CARTESIAN_POINT('',(13.738300751771,53.437062129158,214.5));
#27111=CARTESIAN_POINT('',(13.738300751771,53.437062129158,212.5));
#27112=CARTESIAN_POINT('Origin',(-65.261699248229,29.437062129158,214.5));
#27113=CARTESIAN_POINT('',(-63.661699248229,29.437062129158,212.5));
#27114=CARTESIAN_POINT('',(-63.661699248229,29.437062129158,214.5));
#27115=CARTESIAN_POINT('Origin',(-65.261699248229,29.437062129158,212.5));
#27116=CARTESIAN_POINT('Origin',(65.445980708565,16.608649616242,214.5));
#27117=CARTESIAN_POINT('',(66.6006799111879,16.608649616242,214.5));
#27118=CARTESIAN_POINT('Origin',(65.445980708565,16.608649616242,214.5));
#27119=CARTESIAN_POINT('',(66.6006799111879,16.608649616242,212.5));
#27120=CARTESIAN_POINT('',(66.6006799111879,16.608649616242,214.5));
#27121=CARTESIAN_POINT('Origin',(65.445980708565,16.608649616242,212.5));
#27122=CARTESIAN_POINT('Origin',(-55.2792948506043,10.2688129333875,214.5));
#27123=CARTESIAN_POINT('',(-53.6792948506043,10.2688129333875,212.5));
#27124=CARTESIAN_POINT('',(-53.6792948506043,10.2688129333875,214.5));
#27125=CARTESIAN_POINT('Origin',(-55.2792948506043,10.2688129333875,212.5));
#27126=CARTESIAN_POINT('Origin',(5.7207051493956,10.2688129333875,214.5));
#27127=CARTESIAN_POINT('',(7.3207051493956,10.2688129333875,212.5));
#27128=CARTESIAN_POINT('',(7.3207051493956,10.2688129333875,214.5));
#27129=CARTESIAN_POINT('Origin',(5.7207051493956,10.2688129333875,212.5));
#27130=CARTESIAN_POINT('Origin',(-11.261699248229,29.437062129158,214.5));
#27131=CARTESIAN_POINT('',(-9.66169924822899,29.437062129158,212.5));
#27132=CARTESIAN_POINT('',(-9.66169924822899,29.437062129158,214.5));
#27133=CARTESIAN_POINT('Origin',(-11.261699248229,29.437062129158,212.5));
#27134=CARTESIAN_POINT('Origin',(-5.54425899443339,28.0125156091345,214.5));
#27135=CARTESIAN_POINT('',(-4.21104341383355,28.0125156091345,214.5));
#27136=CARTESIAN_POINT('Origin',(-5.54425899443339,28.0125156091345,214.5));
#27137=CARTESIAN_POINT('',(-4.21104341383355,28.0125156091345,212.5));
#27138=CARTESIAN_POINT('',(-4.21104341383355,28.0125156091345,214.5));
#27139=CARTESIAN_POINT('Origin',(-5.54425899443339,28.0125156091345,212.5));
#27140=CARTESIAN_POINT('Origin',(-1.6080987088528,28.0125156091345,214.5));
#27141=CARTESIAN_POINT('',(-0.287031131713716,28.0125156091345,214.5));
#27142=CARTESIAN_POINT('Origin',(-1.6080987088528,28.0125156091345,214.5));
#27143=CARTESIAN_POINT('',(-0.287031131713716,28.0125156091345,212.5));
#27144=CARTESIAN_POINT('',(-0.287031131713716,28.0125156091345,214.5));
#27145=CARTESIAN_POINT('Origin',(-1.6080987088528,28.0125156091345,212.5));
#27146=CARTESIAN_POINT('Origin',(25.1879034811638,63.7619809501,214.5));
#27147=CARTESIAN_POINT('',(27.2879034811638,63.7619809501,212.5));
#27148=CARTESIAN_POINT('',(27.2879034811638,63.7619809501,214.5));
#27149=CARTESIAN_POINT('Origin',(25.1879034811638,63.7619809501,212.5));
#27150=CARTESIAN_POINT('Origin',(54.6355073401705,34.895083038275,214.5));
#27151=CARTESIAN_POINT('',(56.2355073401705,34.895083038275,212.5));
#27152=CARTESIAN_POINT('',(56.2355073401705,34.895083038275,214.5));
#27153=CARTESIAN_POINT('Origin',(54.6355073401705,34.895083038275,212.5));
#27154=CARTESIAN_POINT('Origin',(39.747079812151,62.1619809501,214.5));
#27155=CARTESIAN_POINT('',(41.347079812151,62.1619809501,212.5));
#27156=CARTESIAN_POINT('',(41.347079812151,62.1619809501,214.5));
#27157=CARTESIAN_POINT('Origin',(39.747079812151,62.1619809501,212.5));
#27158=CARTESIAN_POINT('Origin',(77.738300751771,81.5680647192538,214.5));
#27159=CARTESIAN_POINT('',(79.338300751771,81.5680647192538,212.5));
#27160=CARTESIAN_POINT('',(79.338300751771,81.5680647192538,214.5));
#27161=CARTESIAN_POINT('Origin',(77.738300751771,81.5680647192538,212.5));
#27162=CARTESIAN_POINT('Origin',(73.324673000048,-35.1598100783688,214.5));
#27163=CARTESIAN_POINT('',(74.924673000048,-35.1598100783688,212.5));
#27164=CARTESIAN_POINT('',(74.924673000048,-35.1598100783688,214.5));
#27165=CARTESIAN_POINT('Origin',(73.324673000048,-35.1598100783688,212.5));
#27166=CARTESIAN_POINT('Origin',(40.4592255574045,-7.8397685706167,214.5));
#27167=CARTESIAN_POINT('',(42.0592255574045,-7.8397685706167,212.5));
#27168=CARTESIAN_POINT('',(42.0592255574045,-7.8397685706167,214.5));
#27169=CARTESIAN_POINT('Origin',(40.4592255574045,-7.8397685706167,212.5));
#27170=CARTESIAN_POINT('Origin',(-37.5407744425955,-7.8397685706167,214.5));
#27171=CARTESIAN_POINT('',(-35.9407744425955,-7.8397685706167,212.5));
#27172=CARTESIAN_POINT('',(-35.9407744425955,-7.8397685706167,214.5));
#27173=CARTESIAN_POINT('Origin',(-37.5407744425955,-7.8397685706167,212.5));
#27174=CARTESIAN_POINT('Origin',(-112.45844945829,-38.2430904326252,214.5));
#27175=CARTESIAN_POINT('',(-110.85844945829,-38.2430904326252,212.5));
#27176=CARTESIAN_POINT('',(-110.85844945829,-38.2430904326252,214.5));
#27177=CARTESIAN_POINT('Origin',(-112.45844945829,-38.2430904326252,212.5));
#27178=CARTESIAN_POINT('Origin',(-110.126903127,25.6553383360753,214.5));
#27179=CARTESIAN_POINT('',(-108.526903127,25.6553383360753,212.5));
#27180=CARTESIAN_POINT('',(-108.526903127,25.6553383360753,214.5));
#27181=CARTESIAN_POINT('Origin',(-110.126903127,25.6553383360753,212.5));
#27182=CARTESIAN_POINT('Origin',(-83.761699248229,33.437062129158,214.5));
#27183=CARTESIAN_POINT('',(-83.761699248229,33.437062129158,212.5));
#27184=CARTESIAN_POINT('',(-123.261699248229,33.437062129158,212.5));
#27185=CARTESIAN_POINT('',(-83.761699248229,33.437062129158,212.5));
#27186=CARTESIAN_POINT('',(-123.261699248229,33.437062129158,214.5));
#27187=CARTESIAN_POINT('',(-123.261699248229,33.437062129158,214.5));
#27188=CARTESIAN_POINT('',(-83.761699248229,33.437062129158,214.5));
#27189=CARTESIAN_POINT('',(-83.761699248229,33.437062129158,214.5));
#27190=CARTESIAN_POINT('',(-83.761699248229,33.437062129158,214.5));
#27191=CARTESIAN_POINT('Origin',(-83.761699248229,32.437062129158,214.5));
#27192=CARTESIAN_POINT('',(-83.761699248229,32.437062129158,212.5));
#27193=CARTESIAN_POINT('',(-83.761699248229,32.437062129158,212.5));
#27194=CARTESIAN_POINT('',(-83.761699248229,32.437062129158,214.5));
#27195=CARTESIAN_POINT('',(-83.761699248229,32.437062129158,214.5));
#27196=CARTESIAN_POINT('',(-83.761699248229,32.437062129158,214.5));
#27197=CARTESIAN_POINT('Origin',(4.46549215277239,32.437062129158,214.5));
#27198=CARTESIAN_POINT('',(4.46549215277239,32.437062129158,214.5));
#27199=CARTESIAN_POINT('',(4.46549215277239,32.437062129158,212.5));
#27200=CARTESIAN_POINT('Origin',(13.5853385358292,68.121264388277,214.5));
#27201=CARTESIAN_POINT('',(13.5853385358292,68.121264388277,212.5));
#27202=CARTESIAN_POINT('',(13.5853385358292,68.121264388277,212.5));
#27203=CARTESIAN_POINT('',(13.5853385358292,68.121264388277,214.5));
#27204=CARTESIAN_POINT('',(13.5853385358292,68.121264388277,214.5));
#27205=CARTESIAN_POINT('',(13.5853385358292,68.121264388277,214.5));
#27206=CARTESIAN_POINT('Origin',(20.3202472047774,65.4209130265812,214.5));
#27207=CARTESIAN_POINT('',(18.4696948477504,72.437062129158,212.5));
#27208=CARTESIAN_POINT('Origin',(20.3202472047774,65.4209130265812,212.5));
#27209=CARTESIAN_POINT('',(18.4696948477504,72.437062129158,214.5));
#27210=CARTESIAN_POINT('Origin',(20.3202472047774,65.4209130265812,214.5));
#27211=CARTESIAN_POINT('',(18.4696948477504,72.437062129158,214.5));
#27212=CARTESIAN_POINT('Origin',(44.4912268662385,72.437062129158,214.5));
#27213=CARTESIAN_POINT('',(44.4912268662385,72.437062129158,214.5));
#27214=CARTESIAN_POINT('',(44.4912268662385,72.437062129158,212.5));
#27215=CARTESIAN_POINT('Origin',(66.7028317907535,92.0631475809084,214.5));
#27216=CARTESIAN_POINT('',(66.7028317907535,92.0631475809084,212.5));
#27217=CARTESIAN_POINT('',(66.7028317907535,92.0631475809084,212.5));
#27218=CARTESIAN_POINT('',(66.7028317907535,92.0631475809084,214.5));
#27219=CARTESIAN_POINT('',(66.7028317907535,92.0631475809084,214.5));
#27220=CARTESIAN_POINT('',(66.7028317907535,92.0631475809084,214.5));
#27221=CARTESIAN_POINT('Origin',(72.526950809562,86.133283776482,214.5));
#27222=CARTESIAN_POINT('',(72.1651329632355,94.437062129158,212.5));
#27223=CARTESIAN_POINT('Origin',(72.526950809562,86.133283776482,212.5));
#27224=CARTESIAN_POINT('',(72.1651329632355,94.437062129158,214.5));
#27225=CARTESIAN_POINT('Origin',(72.526950809562,86.133283776482,214.5));
#27226=CARTESIAN_POINT('',(72.1651329632355,94.437062129158,214.5));
#27227=CARTESIAN_POINT('Origin',(82.712821075816,94.437062129158,214.5));
#27228=CARTESIAN_POINT('',(82.712821075816,94.437062129158,212.5));
#27229=CARTESIAN_POINT('',(82.712821075816,94.437062129158,212.5));
#27230=CARTESIAN_POINT('',(82.712821075816,94.437062129158,214.5));
#27231=CARTESIAN_POINT('',(82.712821075816,94.437062129158,214.5));
#27232=CARTESIAN_POINT('',(82.712821075816,94.437062129158,214.5));
#27233=CARTESIAN_POINT('Origin',(82.241473619047,86.8223151727852,214.5));
#27234=CARTESIAN_POINT('',(89.738300751771,88.2379855357732,212.5));
#27235=CARTESIAN_POINT('Origin',(82.241473619047,86.8223151727852,212.5));
#27236=CARTESIAN_POINT('',(89.738300751771,88.2379855357732,214.5));
#27237=CARTESIAN_POINT('Origin',(82.241473619047,86.8223151727852,214.5));
#27238=CARTESIAN_POINT('',(89.738300751771,88.2379855357732,214.5));
#27239=CARTESIAN_POINT('Origin',(89.738300751771,-48.562937870842,214.5));
#27240=CARTESIAN_POINT('',(89.738300751771,-48.562937870842,212.5));
#27241=CARTESIAN_POINT('',(89.738300751771,-48.562937870842,212.5));
#27242=CARTESIAN_POINT('',(89.738300751771,-48.562937870842,214.5));
#27243=CARTESIAN_POINT('',(89.738300751771,-48.562937870842,214.5));
#27244=CARTESIAN_POINT('',(89.738300751771,-48.562937870842,214.5));
#27245=CARTESIAN_POINT('Origin',(67.799693512506,-48.562937870842,214.5));
#27246=CARTESIAN_POINT('',(57.335333187315,-48.562937870842,214.5));
#27247=CARTESIAN_POINT('',(-123.261699248229,-48.562937870842,212.5));
#27248=CARTESIAN_POINT('',(-123.261699248229,-48.562937870842,214.5));
#27249=CARTESIAN_POINT('',(-123.261699248229,-48.562937870842,212.5));
#27250=CARTESIAN_POINT('',(67.799693512506,-48.562937870842,212.5));
#27251=CARTESIAN_POINT('',(67.799693512506,-48.562937870842,214.5));
#27252=CARTESIAN_POINT('',(67.799693512506,-48.562937870842,214.5));
#27253=CARTESIAN_POINT('',(67.799693512506,-48.562937870842,214.5));
#27254=CARTESIAN_POINT('Origin',(67.799693512506,-46.562937870842,214.5));
#27255=CARTESIAN_POINT('',(67.799693512506,-46.562937870842,214.5));
#27256=CARTESIAN_POINT('',(67.799693512506,-46.562937870842,214.5));
#27257=CARTESIAN_POINT('',(67.799693512506,-46.562937870842,214.5));
#27258=CARTESIAN_POINT('Origin',(70.6019681378195,-46.562937870842,214.5));
#27259=CARTESIAN_POINT('',(57.335333187315,-46.562937870842,214.5));
#27260=CARTESIAN_POINT('',(57.335333187315,-46.562937870842,214.5));
#27261=CARTESIAN_POINT('',(70.6019681378195,-46.562937870842,214.5));
#27262=CARTESIAN_POINT('',(70.6019681378195,-46.562937870842,214.5));
#27263=CARTESIAN_POINT('',(70.6019681378195,-46.562937870842,212.5));
#27264=CARTESIAN_POINT('',(70.6019681378195,-46.562937870842,214.5));
#27265=CARTESIAN_POINT('',(76.738300751771,-46.562937870842,212.5));
#27266=CARTESIAN_POINT('',(53.335333187315,-46.562937870842,214.5));
#27267=CARTESIAN_POINT('',(53.335333187315,-46.562937870842,214.5));
#27268=CARTESIAN_POINT('',(57.335333187315,-46.562937870842,214.5));
#27269=CARTESIAN_POINT('Origin',(70.6019681378195,-44.3458473281465,214.5));
#27270=CARTESIAN_POINT('',(70.6019681378195,-44.3458473281465,212.5));
#27271=CARTESIAN_POINT('',(70.6019681378195,-44.3458473281465,212.5));
#27272=CARTESIAN_POINT('',(70.6019681378195,-44.3458473281465,214.5));
#27273=CARTESIAN_POINT('',(70.6019681378195,-44.3458473281465,214.5));
#27274=CARTESIAN_POINT('',(70.6019681378195,-44.3458473281465,214.5));
#27275=CARTESIAN_POINT('Origin',(53.335333187315,-44.3458473281465,214.5));
#27276=CARTESIAN_POINT('',(53.335333187315,-44.3458473281465,212.5));
#27277=CARTESIAN_POINT('',(53.335333187315,-44.3458473281465,212.5));
#27278=CARTESIAN_POINT('',(53.335333187315,-44.3458473281465,214.5));
#27279=CARTESIAN_POINT('',(53.335333187315,-44.3458473281465,214.5));
#27280=CARTESIAN_POINT('',(53.335333187315,-44.3458473281465,214.5));
#27281=CARTESIAN_POINT('Origin',(53.335333187315,-46.562937870842,214.5));
#27282=CARTESIAN_POINT('',(53.335333187315,-46.562937870842,212.5));
#27283=CARTESIAN_POINT('',(53.335333187315,-46.562937870842,214.5));
#27284=CARTESIAN_POINT('Origin',(57.335333187315,-48.562937870842,214.5));
#27285=CARTESIAN_POINT('',(57.335333187315,-48.562937870842,214.5));
#27286=CARTESIAN_POINT('Origin',(-123.261699248229,33.437062129158,214.5));
#27287=CARTESIAN_POINT('',(-123.261699248229,33.437062129158,212.5));
#27288=CARTESIAN_POINT('',(-123.261699248229,33.437062129158,214.5));
#27289=CARTESIAN_POINT('Origin',(82.241473619047,86.8223151727852,212.5));
#27290=CARTESIAN_POINT('Origin',(82.241473619047,86.8223151727852,214.5));
#27291=CARTESIAN_POINT('Origin',(76.738300751771,-46.562937870842,196.5));
#27292=CARTESIAN_POINT('',(76.738300751771,-31.562937870842,196.5));
#27293=CARTESIAN_POINT('Origin',(76.738300751771,-31.562937870842,196.5));
#27294=CARTESIAN_POINT('',(76.738300751771,-31.562937870842,194.5));
#27295=CARTESIAN_POINT('Origin',(76.738300751771,-31.562937870842,194.5));
#27296=CARTESIAN_POINT('',(0.,0.,0.));
#27297=CARTESIAN_POINT('Origin',(-92.5471485639041,33.372246530613,196.800000000001));
#27298=CARTESIAN_POINT('',(-92.3230162611117,33.437062129158,196.800000000001));
#27299=CARTESIAN_POINT('',(-92.7712808666964,33.437062129158,196.800000000001));
#27300=CARTESIAN_POINT('Origin',(-92.5471485639041,33.372246530613,196.800000000001));
#27301=CARTESIAN_POINT('',(-92.3230162611116,33.437062129158,212.500000000001));
#27302=CARTESIAN_POINT('',(-92.3230162611117,33.437062129158,196.800000000001));
#27303=CARTESIAN_POINT('',(-92.7712808666963,33.437062129158,212.500000000001));
#27304=CARTESIAN_POINT('Origin',(-92.547148563904,33.372246530613,212.500000000001));
#27305=CARTESIAN_POINT('',(-92.7712808666964,33.437062129158,196.800000000001));
#27306=CARTESIAN_POINT('Origin',(-77.4703641348207,-5.5271886295165,196.800000000001));
#27307=CARTESIAN_POINT('',(-93.0069996425685,33.437062129158,212.500000000001));
#27308=CARTESIAN_POINT('',(-88.261699248228,-46.062937870842,212.500000000001));
#27309=CARTESIAN_POINT('Origin',(-77.4703641348205,-5.5271886295165,212.500000000001));
#27310=CARTESIAN_POINT('',(-88.2616992482281,-46.062937870842,196.800000000001));
#27311=CARTESIAN_POINT('',(-88.2616992482281,-46.062937870842,196.800000000001));
#27312=CARTESIAN_POINT('',(-93.0069996425686,33.437062129158,196.800000000001));
#27313=CARTESIAN_POINT('Origin',(-77.4703641348207,-5.5271886295165,196.800000000001));
#27314=CARTESIAN_POINT('',(-93.0069996425686,33.437062129158,196.800000000001));
#27315=CARTESIAN_POINT('Origin',(-77.4703641348207,-5.5271886295165,196.800000000001));
#27316=CARTESIAN_POINT('',(-88.2616992482281,33.437062129158,196.800000000001));
#27317=CARTESIAN_POINT('',(-88.2616992482281,33.437062129158,196.800000000001));
#27318=CARTESIAN_POINT('',(-88.2616992482281,33.437062129158,196.800000000001));
#27319=CARTESIAN_POINT('',(-88.2616992482281,33.437062129158,196.800000000001));
#27320=CARTESIAN_POINT('Ctrl Pts',(-131.761699248228,-42.562937870842,201.500000000001));
#27321=CARTESIAN_POINT('Ctrl Pts',(-131.761699248228,-44.562937870842,201.500000000001));
#27322=CARTESIAN_POINT('Ctrl Pts',(-131.761699248228,-44.562937870842,203.500000000001));
#27323=CARTESIAN_POINT('Ctrl Pts',(-131.761699248228,-44.562937870842,205.500000000001));
#27324=CARTESIAN_POINT('Ctrl Pts',(-131.761699248228,-42.562937870842,205.500000000001));
#27325=CARTESIAN_POINT('Ctrl Pts',(-131.761699248228,-40.562937870842,205.500000000001));
#27326=CARTESIAN_POINT('Ctrl Pts',(-131.761699248228,-40.562937870842,203.500000000001));
#27327=CARTESIAN_POINT('Ctrl Pts',(-131.761699248228,-40.562937870842,201.500000000001));
#27328=CARTESIAN_POINT('Ctrl Pts',(-131.761699248228,-42.562937870842,201.500000000001));
#27329=CARTESIAN_POINT('Ctrl Pts',(-132.761699248228,-42.562937870842,201.500000000001));
#27330=CARTESIAN_POINT('Ctrl Pts',(-132.761699248228,-44.562937870842,201.500000000001));
#27331=CARTESIAN_POINT('Ctrl Pts',(-132.761699248228,-44.562937870842,203.500000000001));
#27332=CARTESIAN_POINT('Ctrl Pts',(-132.761699248228,-44.562937870842,205.500000000001));
#27333=CARTESIAN_POINT('Ctrl Pts',(-132.761699248228,-42.562937870842,205.500000000001));
#27334=CARTESIAN_POINT('Ctrl Pts',(-132.761699248228,-40.562937870842,205.500000000001));
#27335=CARTESIAN_POINT('Ctrl Pts',(-132.761699248228,-40.562937870842,203.500000000001));
#27336=CARTESIAN_POINT('Ctrl Pts',(-132.761699248228,-40.562937870842,201.500000000001));
#27337=CARTESIAN_POINT('Ctrl Pts',(-132.761699248228,-42.562937870842,201.500000000001));
#27338=CARTESIAN_POINT('Ctrl Pts',(-132.761699248228,-42.562937870842,202.500000000001));
#27339=CARTESIAN_POINT('Ctrl Pts',(-132.761699248228,-43.562937870842,202.500000000001));
#27340=CARTESIAN_POINT('Ctrl Pts',(-132.761699248228,-43.562937870842,203.500000000001));
#27341=CARTESIAN_POINT('Ctrl Pts',(-132.761699248228,-43.562937870842,204.500000000001));
#27342=CARTESIAN_POINT('Ctrl Pts',(-132.761699248228,-42.562937870842,204.500000000001));
#27343=CARTESIAN_POINT('Ctrl Pts',(-132.761699248228,-41.562937870842,204.500000000001));
#27344=CARTESIAN_POINT('Ctrl Pts',(-132.761699248228,-41.562937870842,203.500000000001));
#27345=CARTESIAN_POINT('Ctrl Pts',(-132.761699248228,-41.562937870842,202.500000000001));
#27346=CARTESIAN_POINT('Ctrl Pts',(-132.761699248228,-42.562937870842,202.500000000001));
#27347=CARTESIAN_POINT('',(-132.761699248228,-42.562937870842,202.500000000001));
#27348=CARTESIAN_POINT('Origin',(-132.761699248228,-42.562937870842,203.500000000001));
#27349=CARTESIAN_POINT('',(-131.761699248228,-42.562937870842,201.500000000001));
#27350=CARTESIAN_POINT('Origin',(-131.761699248228,-42.562937870842,202.500000000001));
#27351=CARTESIAN_POINT('',(-131.761699248228,-42.562937870842,205.500000000001));
#27352=CARTESIAN_POINT('Origin',(-131.761699248228,-42.562937870842,203.500000000001));
#27353=CARTESIAN_POINT('Origin',(-131.761699248228,-42.562937870842,203.500000000001));
#27354=CARTESIAN_POINT('Ctrl Pts',(-131.761699248228,27.437062129158,201.500000000001));
#27355=CARTESIAN_POINT('Ctrl Pts',(-131.761699248228,25.437062129158,201.500000000001));
#27356=CARTESIAN_POINT('Ctrl Pts',(-131.761699248228,25.437062129158,203.500000000001));
#27357=CARTESIAN_POINT('Ctrl Pts',(-131.761699248228,25.437062129158,205.500000000001));
#27358=CARTESIAN_POINT('Ctrl Pts',(-131.761699248228,27.437062129158,205.500000000001));
#27359=CARTESIAN_POINT('Ctrl Pts',(-131.761699248228,29.437062129158,205.500000000001));
#27360=CARTESIAN_POINT('Ctrl Pts',(-131.761699248228,29.437062129158,203.500000000001));
#27361=CARTESIAN_POINT('Ctrl Pts',(-131.761699248228,29.437062129158,201.500000000001));
#27362=CARTESIAN_POINT('Ctrl Pts',(-131.761699248228,27.437062129158,201.500000000001));
#27363=CARTESIAN_POINT('Ctrl Pts',(-132.761699248228,27.437062129158,201.500000000001));
#27364=CARTESIAN_POINT('Ctrl Pts',(-132.761699248228,25.437062129158,201.500000000001));
#27365=CARTESIAN_POINT('Ctrl Pts',(-132.761699248228,25.437062129158,203.500000000001));
#27366=CARTESIAN_POINT('Ctrl Pts',(-132.761699248228,25.437062129158,205.500000000001));
#27367=CARTESIAN_POINT('Ctrl Pts',(-132.761699248228,27.437062129158,205.500000000001));
#27368=CARTESIAN_POINT('Ctrl Pts',(-132.761699248228,29.437062129158,205.500000000001));
#27369=CARTESIAN_POINT('Ctrl Pts',(-132.761699248228,29.437062129158,203.500000000001));
#27370=CARTESIAN_POINT('Ctrl Pts',(-132.761699248228,29.437062129158,201.500000000001));
#27371=CARTESIAN_POINT('Ctrl Pts',(-132.761699248228,27.437062129158,201.500000000001));
#27372=CARTESIAN_POINT('Ctrl Pts',(-132.761699248228,27.437062129158,202.500000000001));
#27373=CARTESIAN_POINT('Ctrl Pts',(-132.761699248228,26.437062129158,202.500000000001));
#27374=CARTESIAN_POINT('Ctrl Pts',(-132.761699248228,26.437062129158,203.500000000001));
#27375=CARTESIAN_POINT('Ctrl Pts',(-132.761699248228,26.437062129158,204.500000000001));
#27376=CARTESIAN_POINT('Ctrl Pts',(-132.761699248228,27.437062129158,204.500000000001));
#27377=CARTESIAN_POINT('Ctrl Pts',(-132.761699248228,28.437062129158,204.500000000001));
#27378=CARTESIAN_POINT('Ctrl Pts',(-132.761699248228,28.437062129158,203.500000000001));
#27379=CARTESIAN_POINT('Ctrl Pts',(-132.761699248228,28.437062129158,202.500000000001));
#27380=CARTESIAN_POINT('Ctrl Pts',(-132.761699248228,27.437062129158,202.500000000001));
#27381=CARTESIAN_POINT('',(-132.761699248228,27.437062129158,202.500000000001));
#27382=CARTESIAN_POINT('Origin',(-132.761699248228,27.437062129158,203.500000000001));
#27383=CARTESIAN_POINT('',(-131.761699248228,27.437062129158,201.500000000001));
#27384=CARTESIAN_POINT('Origin',(-131.761699248228,27.437062129158,202.500000000001));
#27385=CARTESIAN_POINT('',(-131.761699248228,27.437062129158,205.500000000001));
#27386=CARTESIAN_POINT('Origin',(-131.761699248228,27.437062129158,203.500000000001));
#27387=CARTESIAN_POINT('Origin',(-131.761699248228,27.437062129158,203.500000000001));
#27388=CARTESIAN_POINT('Origin',(-132.761699248228,-42.562937870842,203.500000000001));
#27389=CARTESIAN_POINT('Origin',(-132.761699248228,-42.562937870842,203.500000000001));
#27390=CARTESIAN_POINT('',(-123.261699248228,-42.562937870842,205.500000000001));
#27391=CARTESIAN_POINT('Origin',(-123.261699248228,-42.562937870842,203.500000000001));
#27392=CARTESIAN_POINT('',(-132.761699248228,-42.562937870842,205.500000000001));
#27393=CARTESIAN_POINT('Origin',(-132.761699248228,27.437062129158,203.500000000001));
#27394=CARTESIAN_POINT('Origin',(-132.761699248228,27.437062129158,203.500000000001));
#27395=CARTESIAN_POINT('',(-123.261699248228,27.437062129158,205.500000000001));
#27396=CARTESIAN_POINT('Origin',(-123.261699248228,27.437062129158,203.500000000001));
#27397=CARTESIAN_POINT('',(-132.761699248228,27.437062129158,205.500000000001));
#27398=CARTESIAN_POINT('Origin',(-88.261699248228,-48.562937870842,212.500000000001));
#27399=CARTESIAN_POINT('',(-88.261699248228,33.437062129158,212.500000000001));
#27400=CARTESIAN_POINT('Origin',(-88.2616992482281,-48.562937870842,194.500000000001));
#27401=CARTESIAN_POINT('',(-88.2616992482281,33.437062129158,194.500000000001));
#27402=CARTESIAN_POINT('',(-88.2616992482281,-48.562937870842,194.500000000001));
#27403=CARTESIAN_POINT('',(-88.2616992482281,-48.562937870842,194.500000000001));
#27404=CARTESIAN_POINT('',(-123.261699248228,-48.562937870842,194.500000000001));
#27405=CARTESIAN_POINT('',(-88.2616992482281,-48.562937870842,194.500000000001));
#27406=CARTESIAN_POINT('',(-123.261699248228,33.437062129158,194.500000000001));
#27407=CARTESIAN_POINT('',(-123.261699248228,-48.562937870842,194.500000000001));
#27408=CARTESIAN_POINT('',(-88.2616992482281,33.437062129158,194.500000000001));
#27409=CARTESIAN_POINT('Origin',(-123.261699248228,-48.562937870842,194.500000000001));
#27410=CARTESIAN_POINT('',(-123.261699248228,-48.562937870842,212.500000000001));
#27411=CARTESIAN_POINT('',(-123.261699248228,33.437062129158,212.500000000001));
#27412=CARTESIAN_POINT('',(-123.261699248228,-48.562937870842,212.500000000001));
#27413=CARTESIAN_POINT('',(-123.261699248228,33.437062129158,194.500000000001));
#27414=CARTESIAN_POINT('',(-123.261699248228,-48.562937870842,194.500000000001));
#27415=CARTESIAN_POINT('Origin',(-88.2616992482281,-48.562937870842,194.500000000001));
#27416=CARTESIAN_POINT('',(-88.261699248228,-48.562937870842,212.500000000001));
#27417=CARTESIAN_POINT('',(-88.261699248228,-48.562937870842,212.500000000001));
#27418=CARTESIAN_POINT('',(-88.2616992482281,-48.562937870842,194.500000000001));
#27419=CARTESIAN_POINT('Origin',(-88.2616992482281,-48.562937870842,194.500000000001));
#27420=CARTESIAN_POINT('',(-88.261699248228,-48.562937870842,212.500000000001));
#27421=CARTESIAN_POINT('',(-88.2616992482281,33.437062129158,194.500000000001));
#27422=CARTESIAN_POINT('Origin',(-88.2616992482281,33.437062129158,194.500000000001));
#27423=CARTESIAN_POINT('',(-88.261699248228,33.437062129158,212.500000000001));
#27424=CARTESIAN_POINT('Origin',(-88.261699248228,-48.562937870842,212.500000000001));
#27425=CARTESIAN_POINT('',(0.,0.,0.));
#27426=CARTESIAN_POINT('Origin',(-20.4739437433364,34.556757731995,212.621369141518));
#27427=CARTESIAN_POINT('',(-18.4141818172079,35.2822756737311,213.621369141518));
#27428=CARTESIAN_POINT('',(-20.4739437433364,34.556757731995,213.621369141518));
#27429=CARTESIAN_POINT('',(-20.4739437433364,34.556757731995,213.621369141518));
#27430=CARTESIAN_POINT('',(-18.4141818172079,35.2822756737311,212.621369141518));
#27431=CARTESIAN_POINT('',(-18.4141818172079,35.2822756737311,212.621369141518));
#27432=CARTESIAN_POINT('',(-20.4739437433364,34.556757731995,212.621369141518));
#27433=CARTESIAN_POINT('',(-20.4739437433364,34.556757731995,212.621369141518));
#27434=CARTESIAN_POINT('',(-20.4739437433364,34.556757731995,212.621369141518));
#27435=CARTESIAN_POINT('Origin',(-19.9693351501811,33.556757731995,212.621369141518));
#27436=CARTESIAN_POINT('',(-18.4141818172079,33.907356233363,213.621369141518));
#27437=CARTESIAN_POINT('',(-19.9693351501811,33.556757731995,213.621369141518));
#27438=CARTESIAN_POINT('',(-19.9693351501811,33.556757731995,213.621369141518));
#27439=CARTESIAN_POINT('',(-19.9693351501811,33.556757731995,212.621369141518));
#27440=CARTESIAN_POINT('',(-19.9693351501811,33.556757731995,212.621369141518));
#27441=CARTESIAN_POINT('',(-18.4141818172079,33.907356233363,212.621369141518));
#27442=CARTESIAN_POINT('',(-19.9693351501811,33.556757731995,212.621369141518));
#27443=CARTESIAN_POINT('',(-18.4141818172079,33.907356233363,212.621369141518));
#27444=CARTESIAN_POINT('Origin',(-70.8141818172079,34.156757731995,209.227232600396));
#27445=CARTESIAN_POINT('',(-72.4141818172079,34.556757731995,209.227232600396));
#27446=CARTESIAN_POINT('',(-72.4141818172079,34.156757731995,208.827232600396));
#27447=CARTESIAN_POINT('Origin',(-72.4141818172079,34.156757731995,209.227232600396));
#27448=CARTESIAN_POINT('',(-70.8141818172079,34.556757731995,209.227232600396));
#27449=CARTESIAN_POINT('',(-47.969665759339,34.556757731995,209.227232600396));
#27450=CARTESIAN_POINT('',(-70.8141818172079,34.156757731995,208.827232600396));
#27451=CARTESIAN_POINT('Origin',(-70.8141818172079,34.156757731995,209.227232600396));
#27452=CARTESIAN_POINT('',(-70.8141818172079,34.156757731995,208.827232600396));
#27453=CARTESIAN_POINT('Origin',(-47.969665759339,33.956757731995,208.427232600396));
#27454=CARTESIAN_POINT('',(-72.4141818172079,33.956757731995,208.827232600396));
#27455=CARTESIAN_POINT('',(-72.4141818172079,33.556757731995,208.427232600396));
#27456=CARTESIAN_POINT('Origin',(-72.4141818172079,33.956757731995,208.427232600396));
#27457=CARTESIAN_POINT('',(-70.8141818172079,33.956757731995,208.827232600396));
#27458=CARTESIAN_POINT('',(-70.8141818172079,33.956757731995,208.827232600396));
#27459=CARTESIAN_POINT('',(-70.8141818172079,33.556757731995,208.427232600396));
#27460=CARTESIAN_POINT('Origin',(-70.8141818172079,33.956757731995,208.427232600396));
#27461=CARTESIAN_POINT('',(-47.969665759339,33.556757731995,208.427232600396));
#27462=CARTESIAN_POINT('Origin',(-47.969665759339,32.956757731995,209.344010998233));
#27463=CARTESIAN_POINT('',(-70.8141818172079,32.956757731995,209.744010998233));
#27464=CARTESIAN_POINT('',(-70.8141818172079,32.556757731995,209.344010998233));
#27465=CARTESIAN_POINT('Origin',(-70.8141818172079,32.956757731995,209.344010998233));
#27466=CARTESIAN_POINT('',(-72.4141818172079,32.956757731995,209.744010998233));
#27467=CARTESIAN_POINT('',(-70.8141818172079,32.956757731995,209.744010998233));
#27468=CARTESIAN_POINT('',(-72.4141818172079,32.556757731995,209.344010998233));
#27469=CARTESIAN_POINT('Origin',(-72.4141818172079,32.956757731995,209.344010998233));
#27470=CARTESIAN_POINT('',(-72.4141818172079,32.556757731995,209.344010998233));
#27471=CARTESIAN_POINT('Origin',(-70.8141818172079,33.156757731995,210.144010998233));
#27472=CARTESIAN_POINT('',(-70.8141818172079,33.556757731995,210.144010998233));
#27473=CARTESIAN_POINT('',(-70.8141818172079,33.156757731995,209.744010998233));
#27474=CARTESIAN_POINT('Origin',(-70.8141818172079,33.156757731995,210.144010998233));
#27475=CARTESIAN_POINT('',(-72.4141818172079,33.556757731995,210.144010998233));
#27476=CARTESIAN_POINT('',(-47.969665759339,33.556757731995,210.144010998233));
#27477=CARTESIAN_POINT('',(-72.4141818172079,33.156757731995,209.744010998233));
#27478=CARTESIAN_POINT('Origin',(-72.4141818172079,33.156757731995,210.144010998233));
#27479=CARTESIAN_POINT('',(-70.8141818172079,33.156757731995,209.744010998233));
#27480=CARTESIAN_POINT('Origin',(-47.969665759339,33.556757731995,213.621369141518));
#27481=CARTESIAN_POINT('',(-72.4141818172079,33.556757731995,202.621369141518));
#27482=CARTESIAN_POINT('',(-72.4141818172079,33.556757731995,208.827232600396));
#27483=CARTESIAN_POINT('',(-70.8141818172079,33.556757731995,202.621369141518));
#27484=CARTESIAN_POINT('',(-70.8141818172079,33.556757731995,208.827232600396));
#27485=CARTESIAN_POINT('',(-70.8141818172079,33.556757731995,202.621369141518));
#27486=CARTESIAN_POINT('Origin',(-70.8141818172079,33.556757731995,208.827232600396));
#27487=CARTESIAN_POINT('',(-70.8141818172079,33.556757731995,208.827232600396));
#27488=CARTESIAN_POINT('',(-72.4141818172079,33.556757731995,208.827232600396));
#27489=CARTESIAN_POINT('Origin',(-47.969665759339,32.556757731995,213.621369141518));
#27490=CARTESIAN_POINT('',(-70.8141818172079,32.556757731995,202.621369141518));
#27491=CARTESIAN_POINT('',(-70.8141818172079,32.556757731995,202.621369141518));
#27492=CARTESIAN_POINT('',(-72.4141818172079,32.556757731995,202.621369141518));
#27493=CARTESIAN_POINT('',(-72.4141818172079,32.556757731995,202.621369141518));
#27494=CARTESIAN_POINT('',(-70.8141818172079,32.556757731995,202.621369141518));
#27495=CARTESIAN_POINT('Origin',(-70.8141818172079,32.556757731995,209.744010998233));
#27496=CARTESIAN_POINT('',(-70.8141818172079,32.556757731995,209.744010998233));
#27497=CARTESIAN_POINT('',(-72.4141818172079,32.556757731995,209.744010998233));
#27498=CARTESIAN_POINT('Origin',(-47.969665759339,33.556757731995,213.621369141518));
#27499=CARTESIAN_POINT('',(-72.4141818172079,33.556757731995,213.621369141518));
#27500=CARTESIAN_POINT('',(-72.4141818172079,33.556757731995,213.621369141518));
#27501=CARTESIAN_POINT('',(-72.4141818172079,33.556757731995,213.621369141518));
#27502=CARTESIAN_POINT('',(-70.8141818172079,33.556757731995,209.639076092608));
#27503=CARTESIAN_POINT('',(-70.8141818172079,33.556757731995,202.621369141518));
#27504=CARTESIAN_POINT('',(-69.8318887682974,33.556757731995,210.621369141518));
#27505=CARTESIAN_POINT('',(-70.8141818172079,33.556757731995,209.639076092608));
#27506=CARTESIAN_POINT('',(-54.8141818172079,33.556757731995,210.621369141518));
#27507=CARTESIAN_POINT('',(-69.8318887682974,33.556757731995,210.621369141518));
#27508=CARTESIAN_POINT('',(-50.8141818172079,33.556757731995,206.621369141518));
#27509=CARTESIAN_POINT('',(-54.8141818172079,33.556757731995,210.621369141518));
#27510=CARTESIAN_POINT('',(-20.4141818172079,33.556757731995,206.621369141518));
#27511=CARTESIAN_POINT('',(-50.8141818172079,33.556757731995,206.621369141518));
#27512=CARTESIAN_POINT('',(-20.4141818172079,33.556757731995,212.621369141518));
#27513=CARTESIAN_POINT('',(-20.4141818172079,33.556757731995,206.621369141518));
#27514=CARTESIAN_POINT('',(-20.4141818172079,33.556757731995,212.621369141518));
#27515=CARTESIAN_POINT('Origin',(-47.969665759339,34.556757731995,213.621369141518));
#27516=CARTESIAN_POINT('',(-72.4141818172079,34.556757731995,213.621369141518));
#27517=CARTESIAN_POINT('',(-72.4141818172079,34.556757731995,213.621369141518));
#27518=CARTESIAN_POINT('',(-72.4141818172079,34.556757731995,213.621369141518));
#27519=CARTESIAN_POINT('',(-20.4141818172079,34.556757731995,212.621369141518));
#27520=CARTESIAN_POINT('',(-18.4141818172079,34.556757731995,212.621369141518));
#27521=CARTESIAN_POINT('',(-20.4141818172079,34.556757731995,206.621369141518));
#27522=CARTESIAN_POINT('',(-20.4141818172079,34.556757731995,206.621369141518));
#27523=CARTESIAN_POINT('',(-50.8141818172079,34.556757731995,206.621369141518));
#27524=CARTESIAN_POINT('',(-50.8141818172079,34.556757731995,206.621369141518));
#27525=CARTESIAN_POINT('',(-54.8141818172079,34.556757731995,210.621369141518));
#27526=CARTESIAN_POINT('',(-54.8141818172079,34.556757731995,210.621369141518));
#27527=CARTESIAN_POINT('',(-69.8318887682974,34.556757731995,210.621369141518));
#27528=CARTESIAN_POINT('',(-69.8318887682974,34.556757731995,210.621369141518));
#27529=CARTESIAN_POINT('',(-70.8141818172079,34.556757731995,209.639076092608));
#27530=CARTESIAN_POINT('',(-70.8141818172079,34.556757731995,209.639076092608));
#27531=CARTESIAN_POINT('',(-70.8141818172079,34.556757731995,202.621369141518));
#27532=CARTESIAN_POINT('Origin',(-70.8141818172079,34.556757731995,202.621369141518));
#27533=CARTESIAN_POINT('',(-70.8141818172079,34.556757731995,202.621369141518));
#27534=CARTESIAN_POINT('',(-70.8141818172079,34.556757731995,209.639076092608));
#27535=CARTESIAN_POINT('Origin',(-70.8141818172079,34.556757731995,209.639076092608));
#27536=CARTESIAN_POINT('',(-69.8318887682974,34.556757731995,210.621369141518));
#27537=CARTESIAN_POINT('Origin',(-69.8318887682974,34.556757731995,210.621369141518));
#27538=CARTESIAN_POINT('',(-54.8141818172079,34.556757731995,210.621369141518));
#27539=CARTESIAN_POINT('Origin',(-54.8141818172079,34.556757731995,210.621369141518));
#27540=CARTESIAN_POINT('',(-50.8141818172079,34.556757731995,206.621369141518));
#27541=CARTESIAN_POINT('Origin',(-50.8141818172079,34.556757731995,206.621369141518));
#27542=CARTESIAN_POINT('',(-20.4141818172079,34.556757731995,206.621369141518));
#27543=CARTESIAN_POINT('Origin',(-20.4141818172079,34.556757731995,206.621369141518));
#27544=CARTESIAN_POINT('',(-20.4141818172079,34.556757731995,212.621369141518));
#27545=CARTESIAN_POINT('Origin',(-20.4141818172079,34.556757731995,212.621369141518));
#27546=CARTESIAN_POINT('',(-18.4141818172079,34.556757731995,212.621369141518));
#27547=CARTESIAN_POINT('Origin',(-18.4141818172079,34.556757731995,212.621369141518));
#27548=CARTESIAN_POINT('',(-18.4141818172079,34.556757731995,213.621369141518));
#27549=CARTESIAN_POINT('Origin',(-72.4141818172079,34.556757731995,213.621369141518));
#27550=CARTESIAN_POINT('',(-72.4141818172079,34.556757731995,213.621369141518));
#27551=CARTESIAN_POINT('',(-72.4141818172079,34.556757731995,202.621369141518));
#27552=CARTESIAN_POINT('Origin',(-72.4141818172079,34.556757731995,202.621369141518));
#27553=CARTESIAN_POINT('Origin',(-72.4141818172079,34.556757731995,213.621369141518));
#27554=CARTESIAN_POINT('',(0.,0.,0.));
#27555=CARTESIAN_POINT('Origin',(77.215862801455,80.368869783441,212.));
#27556=CARTESIAN_POINT('',(76.8377292359511,78.8141945740679,198.4));
#27557=CARTESIAN_POINT('',(76.8377292359511,78.8141945740679,198.312499998088));
#27558=CARTESIAN_POINT('',(76.8377292359511,78.8141945740678,212.));
#27559=CARTESIAN_POINT('',(76.8377292359511,78.8141945740679,198.1));
#27560=CARTESIAN_POINT('',(76.8377292359511,78.8141945740679,198.006249999044));
#27561=CARTESIAN_POINT('',(76.8768229089103,81.9325359726461,198.1));
#27562=CARTESIAN_POINT('Origin',(77.215862801455,80.368869783441,198.1));
#27563=CARTESIAN_POINT('Ctrl Pts',(76.8377292359512,78.8141945740679,198.4));
#27564=CARTESIAN_POINT('Ctrl Pts',(76.8306919936837,78.8159061968518,198.399542658881));
#27565=CARTESIAN_POINT('Ctrl Pts',(76.8236645970994,78.8176660326881,198.399083409546));
#27566=CARTESIAN_POINT('Ctrl Pts',(76.6110740000279,78.8724418439445,198.385112914876));
#27567=CARTESIAN_POINT('Ctrl Pts',(76.4181464081622,78.9657791947612,198.370237944061));
#27568=CARTESIAN_POINT('Ctrl Pts',(76.0829345406545,79.2199759547389,198.339759359453));
#27569=CARTESIAN_POINT('Ctrl Pts',(75.9429889506103,79.3772603708408,198.324459092766));
#27570=CARTESIAN_POINT('Ctrl Pts',(75.7339714702803,79.7321991446286,198.295564011952));
#27571=CARTESIAN_POINT('Ctrl Pts',(75.6651563328787,79.9254175659732,198.283141851207));
#27572=CARTESIAN_POINT('Ctrl Pts',(75.6018680703669,80.3382054162985,198.254986009091));
#27573=CARTESIAN_POINT('Ctrl Pts',(75.6122792966977,80.5543572171928,198.239492006727));
#27574=CARTESIAN_POINT('Ctrl Pts',(75.7155422448449,80.9617434362757,198.208848757408));
#27575=CARTESIAN_POINT('Ctrl Pts',(75.8042954983089,81.1498759107796,198.193989913992));
#27576=CARTESIAN_POINT('Ctrl Pts',(76.038522207399,81.4687760552142,198.167359146374));
#27577=CARTESIAN_POINT('Ctrl Pts',(76.1769316856716,81.6003554294599,198.155785245017));
#27578=CARTESIAN_POINT('Ctrl Pts',(76.5001429204423,81.8134379281221,198.128799947654));
#27579=CARTESIAN_POINT('Ctrl Pts',(76.6837837988249,81.8906805180791,198.114366048253));
#27580=CARTESIAN_POINT('Ctrl Pts',(76.8768229089103,81.9325359726461,198.1));
#27581=CARTESIAN_POINT('Origin',(77.215862801455,80.368869783441,212.));
#27582=CARTESIAN_POINT('',(76.8377292359509,78.8141945740679,199.1));
#27583=CARTESIAN_POINT('',(76.8377292359516,78.8141945740678,199.012499998088));
#27584=CARTESIAN_POINT('',(76.8377292359511,78.8141945740678,212.));
#27585=CARTESIAN_POINT('Ctrl Pts',(76.8377292359511,78.8141945740679,198.312499998088));
#27586=CARTESIAN_POINT('Ctrl Pts',(76.9720481847989,78.7815250475093,198.321229209914));
#27587=CARTESIAN_POINT('Ctrl Pts',(77.1100034492629,78.7664077184876,198.330572722172));
#27588=CARTESIAN_POINT('Ctrl Pts',(77.3912490807052,78.772083398796,198.350369291815));
#27589=CARTESIAN_POINT('Ctrl Pts',(77.5333074426643,78.7941606892817,198.360762469305));
#27590=CARTESIAN_POINT('Ctrl Pts',(77.8761650962969,78.8957753239252,198.386837255165));
#27591=CARTESIAN_POINT('Ctrl Pts',(78.0675144740926,78.997472028618,198.402311907275));
#27592=CARTESIAN_POINT('Ctrl Pts',(78.3899087615022,79.2630351083584,198.430315976051));
#27593=CARTESIAN_POINT('Ctrl Pts',(78.5206414445282,79.4208075667966,198.442813555558));
#27594=CARTESIAN_POINT('Ctrl Pts',(78.7189000424947,79.7819394290783,198.471816660304));
#27595=CARTESIAN_POINT('Ctrl Pts',(78.7825859666829,79.982896651337,198.487152174499));
#27596=CARTESIAN_POINT('Ctrl Pts',(78.8295412717651,80.4012094693317,198.517599255318));
#27597=CARTESIAN_POINT('Ctrl Pts',(78.8110498611063,80.6147063508936,198.532407084758));
#27598=CARTESIAN_POINT('Ctrl Pts',(78.6942808378984,81.0135564815686,198.558653809128));
#27599=CARTESIAN_POINT('Ctrl Pts',(78.600431543102,81.1961693227667,198.572795109126));
#27600=CARTESIAN_POINT('Ctrl Pts',(78.3443394345243,81.5226463654582,198.602739991542));
#27601=CARTESIAN_POINT('Ctrl Pts',(78.1822431448,81.6614556920644,198.618278331139));
#27602=CARTESIAN_POINT('Ctrl Pts',(77.8161878865673,81.8665246944038,198.647910117927));
#27603=CARTESIAN_POINT('Ctrl Pts',(77.6164722828377,81.9318335405764,198.660757313471));
#27604=CARTESIAN_POINT('Ctrl Pts',(77.2054327727601,81.9820302740299,198.688490755413));
#27605=CARTESIAN_POINT('Ctrl Pts',(76.9981836939206,81.9672995861781,198.703295046626));
#27606=CARTESIAN_POINT('Ctrl Pts',(76.5928838188948,81.8580539426185,198.733895685235));
#27607=CARTESIAN_POINT('Ctrl Pts',(76.3995268294322,81.7614929603439,198.749405529619));
#27608=CARTESIAN_POINT('Ctrl Pts',(76.0704528171171,81.5044202670635,198.777702946476));
#27609=CARTESIAN_POINT('Ctrl Pts',(75.9354522947806,81.349683608691,198.790073141041));
#27610=CARTESIAN_POINT('Ctrl Pts',(75.7282528365861,80.993697573892,198.818865733043));
#27611=CARTESIAN_POINT('Ctrl Pts',(75.6596351655703,80.7949368475463,198.834130610186));
#27612=CARTESIAN_POINT('Ctrl Pts',(75.6018825845919,80.3784602743984,198.864633656738));
#27613=CARTESIAN_POINT('Ctrl Pts',(75.6148283713537,80.1645110358893,198.879569101951));
#27614=CARTESIAN_POINT('Ctrl Pts',(75.7211303911452,79.7630956612239,198.906177950839));
#27615=CARTESIAN_POINT('Ctrl Pts',(75.8099594347692,79.5784884263048,198.919811057053));
#27616=CARTESIAN_POINT('Ctrl Pts',(76.0566259187301,79.2461087993588,198.949556000229));
#27617=CARTESIAN_POINT('Ctrl Pts',(76.2144478184568,79.1033283836519,198.965068839922));
#27618=CARTESIAN_POINT('Ctrl Pts',(76.5332172535871,78.9129289906697,198.991468046714));
#27619=CARTESIAN_POINT('Ctrl Pts',(76.6823153024518,78.8519948968934,199.002399850954));
#27620=CARTESIAN_POINT('Ctrl Pts',(76.837729235952,78.8141945740677,199.012499998088));
#27621=CARTESIAN_POINT('Ctrl Pts',(76.8377292359507,78.814194574068,199.1));
#27622=CARTESIAN_POINT('Ctrl Pts',(76.803254858159,78.822579553332,199.097759555529));
#27623=CARTESIAN_POINT('Ctrl Pts',(76.7690280068441,78.8321188092932,199.095474049025));
#27624=CARTESIAN_POINT('Ctrl Pts',(76.532562538695,78.9066126046754,199.079251543903));
#27625=CARTESIAN_POINT('Ctrl Pts',(76.3447869226595,79.0100914642844,199.064137681813));
#27626=CARTESIAN_POINT('Ctrl Pts',(76.024305592285,79.2811061032762,199.033589251734));
#27627=CARTESIAN_POINT('Ctrl Pts',(75.8934314734524,79.4446211161594,199.018453730095));
#27628=CARTESIAN_POINT('Ctrl Pts',(75.7027394696539,79.8100007830423,198.989999487709));
#27629=CARTESIAN_POINT('Ctrl Pts',(75.6437512894612,80.0078414436886,198.977670895753));
#27630=CARTESIAN_POINT('Ctrl Pts',(75.6026562880355,80.423595255991,198.948922463328));
#27631=CARTESIAN_POINT('Ctrl Pts',(75.6242867916757,80.6377408622658,198.933377264154));
#27632=CARTESIAN_POINT('Ctrl Pts',(75.7477523210465,81.0372197979956,198.902946110429));
#27633=CARTESIAN_POINT('Ctrl Pts',(75.8454052288813,81.219707520826,198.888333839163));
#27634=CARTESIAN_POINT('Ctrl Pts',(76.1078081931828,81.5421385341799,198.860967354125));
#27635=CARTESIAN_POINT('Ctrl Pts',(76.2716666646728,81.6776381830664,198.847571727011));
#27636=CARTESIAN_POINT('Ctrl Pts',(76.6424477897895,81.8773440853991,198.817531960833));
#27637=CARTESIAN_POINT('Ctrl Pts',(76.8456364090363,81.939611578871,198.802037218959));
#27638=CARTESIAN_POINT('Ctrl Pts',(77.2569926218215,81.9811692267037,198.772400501348));
#27639=CARTESIAN_POINT('Ctrl Pts',(77.4608895405315,81.9629520640054,198.759004513137));
#27640=CARTESIAN_POINT('Ctrl Pts',(77.8600269118437,81.8487800120576,198.732204504379));
#27641=CARTESIAN_POINT('Ctrl Pts',(78.0504551467755,81.7503507672924,198.71720498185));
#27642=CARTESIAN_POINT('Ctrl Pts',(78.3784297681607,81.4876632826046,198.686680604441));
#27643=CARTESIAN_POINT('Ctrl Pts',(78.5138862290576,81.3272088530237,198.671457497262));
#27644=CARTESIAN_POINT('Ctrl Pts',(78.7137859745099,80.9670331217066,198.642779630751));
#27645=CARTESIAN_POINT('Ctrl Pts',(78.7777254334594,80.7715523859113,198.630445530054));
#27646=CARTESIAN_POINT('Ctrl Pts',(78.8300314602077,80.3572395924842,198.601992391047));
#27647=CARTESIAN_POINT('Ctrl Pts',(78.8140435325791,80.1420106726523,198.586467674468));
#27648=CARTESIAN_POINT('Ctrl Pts',(78.7007132113641,79.7384164908133,198.555919607586));
#27649=CARTESIAN_POINT('Ctrl Pts',(78.6075117625974,79.5530263026121,198.541178403936));
#27650=CARTESIAN_POINT('Ctrl Pts',(78.353950676021,79.2250085562103,198.513568461787));
#27651=CARTESIAN_POINT('Ctrl Pts',(78.1950310205265,79.0863276432054,198.500556585232));
#27652=CARTESIAN_POINT('Ctrl Pts',(77.8309453443636,78.8768184961485,198.470784351695));
#27653=CARTESIAN_POINT('Ctrl Pts',(77.6289911909212,78.808785940305,198.455257798593));
#27654=CARTESIAN_POINT('Ctrl Pts',(77.2251848651683,78.7569260165313,198.425938172113));
#27655=CARTESIAN_POINT('Ctrl Pts',(77.0279400750016,78.7679308256438,198.41236155226));
#27656=CARTESIAN_POINT('Ctrl Pts',(76.8377292359511,78.8141945740679,198.4));
#27657=CARTESIAN_POINT('Origin',(77.215862801455,80.368869783441,212.));
#27658=CARTESIAN_POINT('',(76.8377292359509,78.8141945740679,199.8));
#27659=CARTESIAN_POINT('',(76.8377292359513,78.8141945740678,199.712499998088));
#27660=CARTESIAN_POINT('',(76.8377292359511,78.8141945740678,212.));
#27661=CARTESIAN_POINT('Ctrl Pts',(76.837729235952,78.8141945740677,199.012499998088));
#27662=CARTESIAN_POINT('Ctrl Pts',(76.8854116654775,78.8025970860652,199.01559881647));
#27663=CARTESIAN_POINT('Ctrl Pts',(76.9336787715119,78.793180648293,199.01878326277));
#27664=CARTESIAN_POINT('Ctrl Pts',(77.1855842440625,78.756024231363,199.035648622212));
#27665=CARTESIAN_POINT('Ctrl Pts',(77.3926167754525,78.7654644547276,199.050329297338));
#27666=CARTESIAN_POINT('Ctrl Pts',(77.7995590980122,78.8639346257316,199.080823951734));
#27667=CARTESIAN_POINT('Ctrl Pts',(77.9948655479242,78.9551114350834,199.096359825612));
#27668=CARTESIAN_POINT('Ctrl Pts',(78.3308066382515,79.203277166845,199.124955160147));
#27669=CARTESIAN_POINT('Ctrl Pts',(78.4702842926093,79.3548996297549,199.137276119643));
#27670=CARTESIAN_POINT('Ctrl Pts',(78.6866319321173,79.7055359348698,199.165847324901));
#27671=CARTESIAN_POINT('Ctrl Pts',(78.7602426169992,79.9019169960723,199.181029643047));
#27672=CARTESIAN_POINT('Ctrl Pts',(78.8290181862994,80.3162153276788,199.21156831412));
#27673=CARTESIAN_POINT('Ctrl Pts',(78.8217807425611,80.530474385319,199.226624080228));
#27674=CARTESIAN_POINT('Ctrl Pts',(78.726245797459,80.9344243060637,199.253598049677));
#27675=CARTESIAN_POINT('Ctrl Pts',(78.6424980783076,81.1211153781538,199.266797489178));
#27676=CARTESIAN_POINT('Ctrl Pts',(78.4053938550654,81.4593741057634,199.296334104196));
#27677=CARTESIAN_POINT('Ctrl Pts',(78.2519971062266,81.6060477692569,199.311809573208));
#27678=CARTESIAN_POINT('Ctrl Pts',(77.8961673620155,81.8324027003303,199.341973775574));
#27679=CARTESIAN_POINT('Ctrl Pts',(77.6970230333772,81.9093834757634,199.355581024474));
#27680=CARTESIAN_POINT('Ctrl Pts',(77.2868111534351,81.9803742875688,199.382830240369));
#27681=CARTESIAN_POINT('Ctrl Pts',(77.0801287919668,81.9762018850526,199.397378413386));
#27682=CARTESIAN_POINT('Ctrl Pts',(76.6718245501323,81.8885129175043,199.427747336064));
#27683=CARTESIAN_POINT('Ctrl Pts',(76.4747143841974,81.8027505106219,199.44329842119));
#27684=CARTESIAN_POINT('Ctrl Pts',(76.1319973254571,81.5635600273011,199.472183898001));
#27685=CARTESIAN_POINT('Ctrl Pts',(75.9880079185057,81.4150152807634,199.484538648629));
#27686=CARTESIAN_POINT('Ctrl Pts',(75.7626694496214,81.069717485316,199.512886550503));
#27687=CARTESIAN_POINT('Ctrl Pts',(75.6842121064397,80.8758026150676,199.527977657111));
#27688=CARTESIAN_POINT('Ctrl Pts',(75.6046455222828,80.4639390682683,199.558529778817));
#27689=CARTESIAN_POINT('Ctrl Pts',(75.6062483704505,80.2495284388588,199.57369338296));
#27690=CARTESIAN_POINT('Ctrl Pts',(75.6911465663229,79.8431810619917,199.601020514144));
#27691=CARTESIAN_POINT('Ctrl Pts',(75.7699483324182,79.6543955980109,199.613878886283));
#27692=CARTESIAN_POINT('Ctrl Pts',(75.997737645633,79.3105102645591,199.643207506063));
#27693=CARTESIAN_POINT('Ctrl Pts',(76.1467436708089,79.1601790240112,199.658635554281));
#27694=CARTESIAN_POINT('Ctrl Pts',(76.4781611250778,78.9363914345893,199.68738292686));
#27695=CARTESIAN_POINT('Ctrl Pts',(76.6533187883288,78.8590475309139,199.700515405639));
#27696=CARTESIAN_POINT('Ctrl Pts',(76.8377292359514,78.8141945740678,199.712499998088));
#27697=CARTESIAN_POINT('Ctrl Pts',(76.8377292359506,78.814194574068,199.8));
#27698=CARTESIAN_POINT('Ctrl Pts',(76.7776741872748,78.8288013739613,199.796097101373));
#27699=CARTESIAN_POINT('Ctrl Pts',(76.7184087914351,78.8469012544151,199.792059976321));
#27700=CARTESIAN_POINT('Ctrl Pts',(76.4610472853451,78.9422062861736,199.773687527242));
#27701=CARTESIAN_POINT('Ctrl Pts',(76.2785728993196,79.054880815752,199.758390268385));
#27702=CARTESIAN_POINT('Ctrl Pts',(75.9725918263895,79.3408108169731,199.727855637987));
#27703=CARTESIAN_POINT('Ctrl Pts',(75.8504158980802,79.5096772799917,199.712909438187));
#27704=CARTESIAN_POINT('Ctrl Pts',(75.676982149273,79.8846035228494,199.684884774663));
#27705=CARTESIAN_POINT('Ctrl Pts',(75.6273887810091,80.0870447359082,199.672341226034));
#27706=CARTESIAN_POINT('Ctrl Pts',(75.6076404521229,80.5052218226292,199.643053242266));
#27707=CARTESIAN_POINT('Ctrl Pts',(75.6398499221955,80.7169201980688,199.627499128428));
#27708=CARTESIAN_POINT('Ctrl Pts',(75.7821746261454,81.1079086270507,199.597344542763));
#27709=CARTESIAN_POINT('Ctrl Pts',(75.8880358148982,81.2845991936081,199.583001555874));
#27710=CARTESIAN_POINT('Ctrl Pts',(76.1672426335115,81.596175520434,199.556114562209));
#27711=CARTESIAN_POINT('Ctrl Pts',(76.3408411165774,81.7254472456341,199.541751069757));
#27712=CARTESIAN_POINT('Ctrl Pts',(76.7242979855457,81.9058138191048,199.511220804094));
#27713=CARTESIAN_POINT('Ctrl Pts',(76.9294188839191,81.956884191104,199.495820409909));
#27714=CARTESIAN_POINT('Ctrl Pts',(77.3412033851244,81.9768040425828,199.466597332834));
#27715=CARTESIAN_POINT('Ctrl Pts',(77.5437899955011,81.947983517883,199.45387847663));
#27716=CARTESIAN_POINT('Ctrl Pts',(77.9364767053395,81.8131073340246,199.426376250234));
#27717=CARTESIAN_POINT('Ctrl Pts',(78.1215613870327,81.704825229225,199.411162474011));
#27718=CARTESIAN_POINT('Ctrl Pts',(78.4346104381944,81.425978658953,199.380611707556));
#27719=CARTESIAN_POINT('Ctrl Pts',(78.560999860468,81.2596317542165,199.365570135878));
#27720=CARTESIAN_POINT('Ctrl Pts',(78.742763478423,80.8892780219466,199.337336357528));
#27721=CARTESIAN_POINT('Ctrl Pts',(78.7969110191719,80.6890886408464,199.324933502818));
#27722=CARTESIAN_POINT('Ctrl Pts',(78.8270160600529,80.2720320582584,199.295903381569));
#27723=CARTESIAN_POINT('Ctrl Pts',(78.7999100530586,80.0590843417189,199.280348696751));
#27724=CARTESIAN_POINT('Ctrl Pts',(78.6666596808023,79.6638718993203,199.250051209934));
#27725=CARTESIAN_POINT('Ctrl Pts',(78.5647355517841,79.4843259782325,199.235573764053));
#27726=CARTESIAN_POINT('Ctrl Pts',(78.2936759395128,79.1674473164975,199.208451492165));
#27727=CARTESIAN_POINT('Ctrl Pts',(78.1248579471808,79.0351226849919,199.194596427885));
#27728=CARTESIAN_POINT('Ctrl Pts',(77.7475358028786,78.8452611117838,199.164300777613));
#27729=CARTESIAN_POINT('Ctrl Pts',(77.5432819887802,78.7887246013366,199.148848993046));
#27730=CARTESIAN_POINT('Ctrl Pts',(77.1671515670854,78.7608898413889,199.12195854748));
#27731=CARTESIAN_POINT('Ctrl Pts',(76.9997653690582,78.7747835765921,199.110530515177));
#27732=CARTESIAN_POINT('Ctrl Pts',(76.8377292359507,78.814194574068,199.1));
#27733=CARTESIAN_POINT('Origin',(77.215862801455,80.368869783441,212.));
#27734=CARTESIAN_POINT('',(76.8377292359511,78.8141945740679,200.5));
#27735=CARTESIAN_POINT('',(76.8377292359511,78.8141945740679,200.412499998088));
#27736=CARTESIAN_POINT('',(76.8377292359511,78.8141945740678,212.));
#27737=CARTESIAN_POINT('Ctrl Pts',(76.8377292359514,78.8141945740678,199.712499998088));
#27738=CARTESIAN_POINT('Ctrl Pts',(76.8601595856551,78.8087389856222,199.713957717014));
#27739=CARTESIAN_POINT('Ctrl Pts',(76.8827246653436,78.8037647658874,199.715434732537));
#27740=CARTESIAN_POINT('Ctrl Pts',(77.1059319935505,78.7596160590715,199.730148581308));
#27741=CARTESIAN_POINT('Ctrl Pts',(77.3121533169625,78.7587557394075,199.744561314105));
#27742=CARTESIAN_POINT('Ctrl Pts',(77.7215015090649,78.8360958232994,199.774791118394));
#27743=CARTESIAN_POINT('Ctrl Pts',(77.920205761451,78.9166352832053,199.790346671055));
#27744=CARTESIAN_POINT('Ctrl Pts',(78.2693460365696,79.1471396865218,199.819503534684));
#27745=CARTESIAN_POINT('Ctrl Pts',(78.4176997359322,79.2927498245599,199.831966567357));
#27746=CARTESIAN_POINT('Ctrl Pts',(78.6515343010296,79.6329329489428,199.86009849949));
#27747=CARTESIAN_POINT('Ctrl Pts',(78.7345089081834,79.8244045688921,199.875094343593));
#27748=CARTESIAN_POINT('Ctrl Pts',(78.8242168733294,80.2337018624852,199.905639406342));
#27749=CARTESIAN_POINT('Ctrl Pts',(78.8279518622446,80.4481151143427,199.920895181364));
#27750=CARTESIAN_POINT('Ctrl Pts',(78.7531522647425,80.8566382418602,199.948550492446));
#27751=CARTESIAN_POINT('Ctrl Pts',(78.6789862693489,81.0474474543987,199.961163870517));
#27752=CARTESIAN_POINT('Ctrl Pts',(78.459921675685,81.3965165483435,199.990293326169));
#27753=CARTESIAN_POINT('Ctrl Pts',(78.3150937441767,81.5501499381234,200.005667272635));
#27754=CARTESIAN_POINT('Ctrl Pts',(77.9719250383511,81.7948674721432,200.036088247044));
#27755=CARTESIAN_POINT('Ctrl Pts',(77.7762937142079,81.8824471403564,200.050586284423));
#27756=CARTESIAN_POINT('Ctrl Pts',(77.3705955233945,81.9743643288998,200.077090629358));
#27757=CARTESIAN_POINT('Ctrl Pts',(77.1650557512591,81.9809886005648,200.091337500084));
#27758=CARTESIAN_POINT('Ctrl Pts',(76.7548241561411,81.9155604084609,200.121384907449));
#27759=CARTESIAN_POINT('Ctrl Pts',(76.5544508890402,81.8410637828125,200.136933361737));
#27760=CARTESIAN_POINT('Ctrl Pts',(76.1980154936663,81.6206631837517,200.166393558143));
#27761=CARTESIAN_POINT('Ctrl Pts',(76.044579685092,81.4784120954065,200.179072034181));
#27762=CARTESIAN_POINT('Ctrl Pts',(75.8011131179273,81.1441180710667,200.20695270211));
#27763=CARTESIAN_POINT('Ctrl Pts',(75.7130966242145,80.9555460879553,200.221829988864));
#27764=CARTESIAN_POINT('Ctrl Pts',(75.6114955338623,80.5475615615859,200.252486990691));
#27765=CARTESIAN_POINT('Ctrl Pts',(75.6020022505719,80.3312717497537,200.267974952688));
#27766=CARTESIAN_POINT('Ctrl Pts',(75.6670900122648,79.9187442358169,200.29608133955));
#27767=CARTESIAN_POINT('Ctrl Pts',(75.7367070491808,79.7258918308971,200.308525861151));
#27768=CARTESIAN_POINT('Ctrl Pts',(75.9472279372274,79.3718247070364,200.337456348369));
#27769=CARTESIAN_POINT('Ctrl Pts',(76.0879086041414,79.2150761562445,200.352768404332));
#27770=CARTESIAN_POINT('Ctrl Pts',(76.4242954096651,78.9623022207994,200.383237319686));
#27771=CARTESIAN_POINT('Ctrl Pts',(76.6176225724446,78.8698127731646,200.398090673413));
#27772=CARTESIAN_POINT('Ctrl Pts',(76.8281845736508,78.8165393565164,200.41187853009));
#27773=CARTESIAN_POINT('Ctrl Pts',(76.8329546462495,78.8153558665467,200.412189703783));
#27774=CARTESIAN_POINT('Ctrl Pts',(76.8377292359511,78.8141945740679,200.412499998088));
#27775=CARTESIAN_POINT('Ctrl Pts',(76.8377292359511,78.8141945740679,200.5));
#27776=CARTESIAN_POINT('Ctrl Pts',(76.7505355862406,78.8354021198341,200.494333399385));
#27777=CARTESIAN_POINT('Ctrl Pts',(76.6651008066216,78.8639490172179,200.488390033652));
#27778=CARTESIAN_POINT('Ctrl Pts',(76.3862547297379,78.9841881185334,200.467629017513));
#27779=CARTESIAN_POINT('Ctrl Pts',(76.2091073795797,79.1071214080758,200.452096196954));
#27780=CARTESIAN_POINT('Ctrl Pts',(75.919134425438,79.4093510209623,200.421585198431));
#27781=CARTESIAN_POINT('Ctrl Pts',(75.8067701191103,79.5835831991175,200.40688632741));
#27782=CARTESIAN_POINT('Ctrl Pts',(75.6525829641113,79.9688219410575,200.379357548924));
#27783=CARTESIAN_POINT('Ctrl Pts',(75.6136850892892,80.1766846348362,200.366226292963));
#27784=CARTESIAN_POINT('Ctrl Pts',(75.6182428396301,80.5970629377492,200.336363492498));
#27785=CARTESIAN_POINT('Ctrl Pts',(75.6621865959909,80.8053862221654,200.320846294675));
#27786=CARTESIAN_POINT('Ctrl Pts',(75.8252971031959,81.1859474327836,200.29107229427));
#27787=CARTESIAN_POINT('Ctrl Pts',(75.9401458805879,81.3556580291316,200.277371065842));
#27788=CARTESIAN_POINT('Ctrl Pts',(76.233558924232,81.6495534276981,200.250814105619));
#27789=CARTESIAN_POINT('Ctrl Pts',(76.4119220403041,81.7684056311527,200.235896453611));
#27790=CARTESIAN_POINT('Ctrl Pts',(76.8009446034018,81.9281170529271,200.205400191864));
#27791=CARTESIAN_POINT('Ctrl Pts',(77.0073123858077,81.9688481803144,200.19012451813));
#27792=CARTESIAN_POINT('Ctrl Pts',(77.4192074068678,81.968890864281,200.161301221737));
#27793=CARTESIAN_POINT('Ctrl Pts',(77.6207820272753,81.9301026773435,200.14891743278));
#27794=CARTESIAN_POINT('Ctrl Pts',(78.0085391862507,81.7751067411898,200.120662184743));
#27795=CARTESIAN_POINT('Ctrl Pts',(78.1893481759911,81.6565546605442,200.105156831585));
#27796=CARTESIAN_POINT('Ctrl Pts',(78.4877824315008,81.3611459774882,200.074542992852));
#27797=CARTESIAN_POINT('Ctrl Pts',(78.6048141413239,81.1893810893234,200.059722177943));
#27798=CARTESIAN_POINT('Ctrl Pts',(78.7681363382764,80.8089933634251,200.031955840391));
#27799=CARTESIAN_POINT('Ctrl Pts',(78.8121438676005,80.603740298022,200.019148982569));
#27800=CARTESIAN_POINT('Ctrl Pts',(78.8191876057905,80.1843363761557,199.989555142443));
#27801=CARTESIAN_POINT('Ctrl Pts',(78.7807999465509,79.9743261369516,199.974014168319));
#27802=CARTESIAN_POINT('Ctrl Pts',(78.6275505276573,79.588778510458,199.944056807623));
#27803=CARTESIAN_POINT('Ctrl Pts',(78.5169813912986,79.4156945765352,199.929888224154));
#27804=CARTESIAN_POINT('Ctrl Pts',(78.2309703296968,79.114066650814,199.903588830355));
#27805=CARTESIAN_POINT('Ctrl Pts',(78.0557946210714,78.9906074099691,199.888851074689));
#27806=CARTESIAN_POINT('Ctrl Pts',(77.6703909382835,78.8206350131503,199.858397677972));
#27807=CARTESIAN_POINT('Ctrl Pts',(77.4646014622763,78.7745778735927,199.843053279394));
#27808=CARTESIAN_POINT('Ctrl Pts',(77.1147609741259,78.7658493783967,199.818394185781));
#27809=CARTESIAN_POINT('Ctrl Pts',(76.9742473029973,78.7809901702562,199.808872129625));
#27810=CARTESIAN_POINT('Ctrl Pts',(76.8377292359505,78.814194574068,199.8));
#27811=CARTESIAN_POINT('Origin',(77.215862801455,80.368869783441,212.));
#27812=CARTESIAN_POINT('',(76.8377292359512,78.8141945740679,201.2));
#27813=CARTESIAN_POINT('',(76.8377292359509,78.8141945740679,201.112499998088));
#27814=CARTESIAN_POINT('',(76.8377292359511,78.8141945740678,212.));
#27815=CARTESIAN_POINT('Ctrl Pts',(76.8377292359511,78.8141945740679,200.412499998088));
#27816=CARTESIAN_POINT('Ctrl Pts',(77.0302999172219,78.7673568565296,200.42501491339));
#27817=CARTESIAN_POINT('Ctrl Pts',(77.2300555439046,78.7566661871331,200.438773669814));
#27818=CARTESIAN_POINT('Ctrl Pts',(77.6361104560006,78.8106757494655,200.468294712584));
#27819=CARTESIAN_POINT('Ctrl Pts',(77.8378433339808,78.8796670859991,200.483825438466));
#27820=CARTESIAN_POINT('Ctrl Pts',(78.2008039851846,79.0907979449742,200.513552195936));
#27821=CARTESIAN_POINT('Ctrl Pts',(78.3589068259797,79.2300077242772,200.526508063946));
#27822=CARTESIAN_POINT('Ctrl Pts',(78.6109832588704,79.5589553219541,200.554158302549));
#27823=CARTESIAN_POINT('Ctrl Pts',(78.703428825977,79.7448224249829,200.568920270287));
#27824=CARTESIAN_POINT('Ctrl Pts',(78.8150442280174,80.1490831036783,200.599486006593));
#27825=CARTESIAN_POINT('Ctrl Pts',(78.8300802458321,80.3644798764053,200.615006211804));
#27826=CARTESIAN_POINT('Ctrl Pts',(78.7758931794791,80.778539343366,200.643408987059));
#27827=CARTESIAN_POINT('Ctrl Pts',(78.7111206404444,80.9736291058694,200.655752309459));
#27828=CARTESIAN_POINT('Ctrl Pts',(78.5096661593118,81.332917790401,200.684467514317));
#27829=CARTESIAN_POINT('Ctrl Pts',(78.3734406131165,81.4928414257531,200.699704459788));
#27830=CARTESIAN_POINT('Ctrl Pts',(78.0442186723007,81.7540980926201,200.730222583063));
#27831=CARTESIAN_POINT('Ctrl Pts',(77.8533551387306,81.8516653507143,200.745201663778));
#27832=CARTESIAN_POINT('Ctrl Pts',(77.4536802563094,81.9640479505271,200.771939924285));
#27833=CARTESIAN_POINT('Ctrl Pts',(77.2496582900372,81.9813454348773,200.785410107944));
#27834=CARTESIAN_POINT('Ctrl Pts',(76.8383554720865,81.9378904779783,200.815081987171));
#27835=CARTESIAN_POINT('Ctrl Pts',(76.6353644890328,81.8746461163417,200.83058292681));
#27836=CARTESIAN_POINT('Ctrl Pts',(76.2657096289213,81.6732724609816,200.860578074065));
#27837=CARTESIAN_POINT('Ctrl Pts',(76.1026914420365,81.5372332627568,200.873903071189));
#27838=CARTESIAN_POINT('Ctrl Pts',(75.841776819832,81.2138559265676,200.901310956148));
#27839=CARTESIAN_POINT('Ctrl Pts',(75.7448670750718,81.0308722814056,200.915945557379));
#27840=CARTESIAN_POINT('Ctrl Pts',(75.6230979451896,80.630683292351,200.946397785694));
#27841=CARTESIAN_POINT('Ctrl Pts',(75.602413902907,80.4163453535111,200.961940301802));
#27842=CARTESIAN_POINT('Ctrl Pts',(75.6453970655154,80.0008258998951,200.99063959164));
#27843=CARTESIAN_POINT('Ctrl Pts',(75.7052176842617,79.8033862428561,201.002963231553));
#27844=CARTESIAN_POINT('Ctrl Pts',(75.8974535098298,79.4388732188919,201.031455263981));
#27845=CARTESIAN_POINT('Ctrl Pts',(76.0290990402504,79.2758614084399,201.046606135839));
#27846=CARTESIAN_POINT('Ctrl Pts',(76.3508490844663,79.0062252356137,201.077152076056));
#27847=CARTESIAN_POINT('Ctrl Pts',(76.5390782250257,78.9035862586545,201.092247570537));
#27848=CARTESIAN_POINT('Ctrl Pts',(76.7735964358505,78.8308509783593,201.108278832138));
#27849=CARTESIAN_POINT('Ctrl Pts',(76.8055554972657,78.8220199838071,201.110409069127));
#27850=CARTESIAN_POINT('Ctrl Pts',(76.8377292359507,78.814194574068,201.112499998088));
#27851=CARTESIAN_POINT('Ctrl Pts',(76.8377292359512,78.8141945740679,201.2));
#27852=CARTESIAN_POINT('Ctrl Pts',(76.7230577379177,78.8420853786241,201.192547650162));
#27853=CARTESIAN_POINT('Ctrl Pts',(76.6115947990365,78.8826276152677,201.184627535099));
#27854=CARTESIAN_POINT('Ctrl Pts',(76.3150545531594,79.0295937708904,201.161587591416));
#27855=CARTESIAN_POINT('Ctrl Pts',(76.145434372447,79.1608629281559,201.146032066305));
#27856=CARTESIAN_POINT('Ctrl Pts',(75.8726108484588,79.4758742834271,201.115782018085));
#27857=CARTESIAN_POINT('Ctrl Pts',(75.7696103415582,79.6546125310239,201.101350139248));
#27858=CARTESIAN_POINT('Ctrl Pts',(75.6336972630993,80.0493201135081,201.074308430542));
#27859=CARTESIAN_POINT('Ctrl Pts',(75.6052336851466,80.2625778233924,201.060286307551));
#27860=CARTESIAN_POINT('Ctrl Pts',(75.6333440080259,80.6844893975392,201.029908999931));
#27861=CARTESIAN_POINT('Ctrl Pts',(75.6882924470039,80.8889797296278,201.014473731096));
#27862=CARTESIAN_POINT('Ctrl Pts',(75.8708941126286,81.2589254386447,200.985115966184));
#27863=CARTESIAN_POINT('Ctrl Pts',(75.9943880638178,81.4220094854326,200.972215147236));
#27864=CARTESIAN_POINT('Ctrl Pts',(76.3028196954746,81.6998287002969,200.944936846831));
#27865=CARTESIAN_POINT('Ctrl Pts',(76.4873000683498,81.8090966564369,200.929787631469));
#27866=CARTESIAN_POINT('Ctrl Pts',(76.8833265687373,81.9475986645516,200.899236095611));
#27867=CARTESIAN_POINT('Ctrl Pts',(77.0904587978782,81.9773666558241,200.884131691749));
#27868=CARTESIAN_POINT('Ctrl Pts',(77.5021859648924,81.9563251671592,200.855752400869));
#27869=CARTESIAN_POINT('Ctrl Pts',(77.7028802441797,81.9066637066071,200.84340722707));
#27870=CARTESIAN_POINT('Ctrl Pts',(78.0820047419905,81.7309075887329,200.814562023466));
#27871=CARTESIAN_POINT('Ctrl Pts',(78.2553693071718,81.6036784189801,200.799012421272));
#27872=CARTESIAN_POINT('Ctrl Pts',(78.536684912461,81.2948279961493,200.768624678923));
#27873=CARTESIAN_POINT('Ctrl Pts',(78.6443066654089,81.1182412310875,200.754057389924));
#27874=CARTESIAN_POINT('Ctrl Pts',(78.7892343581798,80.7281654087846,200.726773434395));
#27875=CARTESIAN_POINT('Ctrl Pts',(78.8228831626828,80.5175960494746,200.713230635708));
#27876=CARTESIAN_POINT('Ctrl Pts',(78.8064479126939,80.0963686544912,200.683102995361));
#27877=CARTESIAN_POINT('Ctrl Pts',(78.7569066916746,79.8899114757666,200.667621554002));
#27878=CARTESIAN_POINT('Ctrl Pts',(78.5839060893216,79.5146866365054,200.638055208749));
#27879=CARTESIAN_POINT('Ctrl Pts',(78.4647172737818,79.3483417121807,200.624799640214));
#27880=CARTESIAN_POINT('Ctrl Pts',(78.1637244074197,79.0624835874737,200.597877057872));
#27881=CARTESIAN_POINT('Ctrl Pts',(77.9822244022444,78.9484014966514,200.582837696619));
#27882=CARTESIAN_POINT('Ctrl Pts',(77.5895403317286,78.7992995627259,200.552302732084));
#27883=CARTESIAN_POINT('Ctrl Pts',(77.3827169839753,78.7640755952016,200.537108085843));
#27884=CARTESIAN_POINT('Ctrl Pts',(77.0609849749371,78.7723096416387,200.514763647388));
#27885=CARTESIAN_POINT('Ctrl Pts',(76.9479785400891,78.7873793510447,200.507164957273));
#27886=CARTESIAN_POINT('Ctrl Pts',(76.8377292359511,78.8141945740679,200.5));
#27887=CARTESIAN_POINT('Origin',(77.215862801455,80.368869783441,212.));
#27888=CARTESIAN_POINT('',(76.8377292359515,78.8141945740678,201.9));
#27889=CARTESIAN_POINT('',(76.8377292359509,78.814194574068,201.812499998088));
#27890=CARTESIAN_POINT('',(76.8377292359511,78.8141945740678,212.));
#27891=CARTESIAN_POINT('Ctrl Pts',(76.8377292359507,78.814194574068,201.112499998088));
#27892=CARTESIAN_POINT('Ctrl Pts',(77.002096180345,78.7742166684835,201.123181989625));
#27893=CARTESIAN_POINT('Ctrl Pts',(77.1719446163093,78.7605016544631,201.134785981505));
#27894=CARTESIAN_POINT('Ctrl Pts',(77.5504206323416,78.7902082684024,201.161878936476));
#27895=CARTESIAN_POINT('Ctrl Pts',(77.7545082243137,78.8476990344998,201.177338653418));
#27896=CARTESIAN_POINT('Ctrl Pts',(78.1307490414463,79.0392072412851,201.207592396316));
#27897=CARTESIAN_POINT('Ctrl Pts',(78.2987375993833,79.1720620104365,201.22136567213));
#27898=CARTESIAN_POINT('Ctrl Pts',(78.5683643434518,79.4898654486178,201.248528773316));
#27899=CARTESIAN_POINT('Ctrl Pts',(78.6695876376196,79.669904966601,201.263029113832));
#27900=CARTESIAN_POINT('Ctrl Pts',(78.8012283126906,80.0658395556713,201.293350026175));
#27901=CARTESIAN_POINT('Ctrl Pts',(78.827431612851,80.2789948332638,201.308903860888));
#27902=CARTESIAN_POINT('Ctrl Pts',(78.7955064913181,80.6958435296877,201.337887888365));
#27903=CARTESIAN_POINT('Ctrl Pts',(78.7405579756507,80.8956412160388,201.350273062725));
#27904=CARTESIAN_POINT('Ctrl Pts',(78.5573221803279,81.2651798560001,201.378543447957));
#27905=CARTESIAN_POINT('Ctrl Pts',(78.4301908339087,81.4310691246104,201.393601108851));
#27906=CARTESIAN_POINT('Ctrl Pts',(78.1159056736257,81.7086411578001,201.424152898562));
#27907=CARTESIAN_POINT('Ctrl Pts',(77.9303695077314,81.8161378845038,201.439350943838));
#27908=CARTESIAN_POINT('Ctrl Pts',(77.5371465566135,81.9493450651334,201.466797419545));
#27909=CARTESIAN_POINT('Ctrl Pts',(77.334463519329,81.9773124642208,201.479558530659));
#27910=CARTESIAN_POINT('Ctrl Pts',(76.9227011821081,81.955669202413,201.508815389526));
#27911=CARTESIAN_POINT('Ctrl Pts',(76.7177123438531,81.9037039845092,201.524224888581));
#27912=CARTESIAN_POINT('Ctrl Pts',(76.3352528979562,81.7217753955709,201.554717383265));
#27913=CARTESIAN_POINT('Ctrl Pts',(76.1624405071601,81.5920017264536,201.568993031485));
#27914=CARTESIAN_POINT('Ctrl Pts',(75.8845606754058,81.2795566083094,201.595918712456));
#27915=CARTESIAN_POINT('Ctrl Pts',(75.7793351114691,81.1023953983769,201.610284091439));
#27916=CARTESIAN_POINT('Ctrl Pts',(75.638479124803,80.7107054391281,201.640463071394));
#27917=CARTESIAN_POINT('Ctrl Pts',(75.6070973802606,80.4987956067845,201.656017903278));
#27918=CARTESIAN_POINT('Ctrl Pts',(75.6285334890446,80.0807938260092,201.685264381511));
#27919=CARTESIAN_POINT('Ctrl Pts',(75.678868774513,79.8787221716487,201.697780400931));
#27920=CARTESIAN_POINT('Ctrl Pts',(75.8536545843852,79.5045335824848,201.725839235094));
#27921=CARTESIAN_POINT('Ctrl Pts',(75.9765160923403,79.3360679972547,201.740801410109));
#27922=CARTESIAN_POINT('Ctrl Pts',(76.2836526802474,79.0512728270737,201.771339847148));
#27923=CARTESIAN_POINT('Ctrl Pts',(76.4665570818323,78.9393052211639,201.786624192886));
#27924=CARTESIAN_POINT('Ctrl Pts',(76.7223422222199,78.8457039354087,201.804827717795));
#27925=CARTESIAN_POINT('Ctrl Pts',(76.7796681677926,78.8283163910155,201.808726685632));
#27926=CARTESIAN_POINT('Ctrl Pts',(76.8377292359506,78.814194574068,201.812499998088));
#27927=CARTESIAN_POINT('Ctrl Pts',(76.8377292359518,78.8141945740677,201.9));
#27928=CARTESIAN_POINT('Ctrl Pts',(76.6938364518796,78.8491926824594,201.890648597215));
#27929=CARTESIAN_POINT('Ctrl Pts',(76.5552610660449,78.9040450255853,201.880577997498));
#27930=CARTESIAN_POINT('Ctrl Pts',(76.2422647744921,79.081730899832,201.855123399538));
#27931=CARTESIAN_POINT('Ctrl Pts',(76.0810339803901,79.2213617176755,201.83958934672));
#27932=CARTESIAN_POINT('Ctrl Pts',(75.8268666155398,79.5490530352132,201.809684842051));
#27933=CARTESIAN_POINT('Ctrl Pts',(75.7340437538269,79.7320686383392,201.795653719495));
#27934=CARTESIAN_POINT('Ctrl Pts',(75.6194005766882,80.1314477387972,201.769332883082));
#27935=CARTESIAN_POINT('Ctrl Pts',(75.6020347944844,80.3450485525558,201.754498292373));
#27936=CARTESIAN_POINT('Ctrl Pts',(75.6511887998393,80.7630110843104,201.724038140283));
#27937=CARTESIAN_POINT('Ctrl Pts',(75.7158822734928,80.9635317136401,201.708716196424));
#27938=CARTESIAN_POINT('Ctrl Pts',(75.9159605933464,81.3236228721634,201.679755468037));
#27939=CARTESIAN_POINT('Ctrl Pts',(76.0475536142187,81.4807778326205,201.667290032282));
#27940=CARTESIAN_POINT('Ctrl Pts',(76.3713046110635,81.7446297174043,201.639226109827));
#27941=CARTESIAN_POINT('Ctrl Pts',(76.5630703759829,81.8452914457543,201.623743539663));
#27942=CARTESIAN_POINT('Ctrl Pts',(76.9669225350538,81.9627811359546,201.593075188823));
#27943=CARTESIAN_POINT('Ctrl Pts',(77.1742465913147,81.9815766866632,201.57818231474));
#27944=CARTESIAN_POINT('Ctrl Pts',(77.5855274997963,81.9393036158957,201.550269532907));
#27945=CARTESIAN_POINT('Ctrl Pts',(77.7854828963734,81.8783259652217,201.537623765747));
#27946=CARTESIAN_POINT('Ctrl Pts',(78.1552306389973,81.6812882661153,201.508201599785));
#27947=CARTESIAN_POINT('Ctrl Pts',(78.3204990159484,81.5455685634545,201.492651517212));
#27948=CARTESIAN_POINT('Ctrl Pts',(78.5835421545281,81.2238498476462,201.462579599162));
#27949=CARTESIAN_POINT('Ctrl Pts',(78.6812562225632,81.0428178170226,201.448311049676));
#27950=CARTESIAN_POINT('Ctrl Pts',(78.8059193648389,80.6458649932158,201.421749644208));
#27951=CARTESIAN_POINT('Ctrl Pts',(78.8286320400919,80.4327224343105,201.40731631648));
#27952=CARTESIAN_POINT('Ctrl Pts',(78.7897393059797,80.0129571686907,201.376905267632));
#27953=CARTESIAN_POINT('Ctrl Pts',(78.7297737453715,79.810440723342,201.361523392513));
#27954=CARTESIAN_POINT('Ctrl Pts',(78.5382070845839,79.4455108789494,201.332366516426));
#27955=CARTESIAN_POINT('Ctrl Pts',(78.4106033162836,79.2854683330141,201.319724000473));
#27956=CARTESIAN_POINT('Ctrl Pts',(78.0951581589779,79.0153745405877,201.292113311217));
#27957=CARTESIAN_POINT('Ctrl Pts',(77.9079624449768,78.9107650324366,201.276869595192));
#27958=CARTESIAN_POINT('Ctrl Pts',(77.5090217545997,78.7824226778875,201.246322427869));
#27959=CARTESIAN_POINT('Ctrl Pts',(77.3017272868094,78.7578419437744,201.231313018556));
#27960=CARTESIAN_POINT('Ctrl Pts',(77.0083879813496,78.7799767627696,201.211240352658));
#27961=CARTESIAN_POINT('Ctrl Pts',(76.9222038524457,78.7936483611116,201.205489894223));
#27962=CARTESIAN_POINT('Ctrl Pts',(76.8377292359512,78.8141945740679,201.2));
#27963=CARTESIAN_POINT('Origin',(77.215862801455,80.368869783441,212.));
#27964=CARTESIAN_POINT('',(76.8377292359514,78.8141945740678,202.6));
#27965=CARTESIAN_POINT('',(76.8377292359511,78.8141945740679,202.512499998088));
#27966=CARTESIAN_POINT('',(76.8377292359511,78.8141945740678,212.));
#27967=CARTESIAN_POINT('Ctrl Pts',(76.8377292359506,78.814194574068,201.812499998088));
#27968=CARTESIAN_POINT('Ctrl Pts',(76.9762100022262,78.7805127956555,201.821499680955));
#27969=CARTESIAN_POINT('Ctrl Pts',(77.1187852308018,78.7654218067803,201.831167015972));
#27970=CARTESIAN_POINT('Ctrl Pts',(77.4706856299835,78.7755288147092,201.855998513953));
#27971=CARTESIAN_POINT('Ctrl Pts',(77.6763755253127,78.8223938236945,201.871352506997));
#27972=CARTESIAN_POINT('Ctrl Pts',(78.0611875659895,78.9939077323625,201.901796106966));
#27973=CARTESIAN_POINT('Ctrl Pts',(78.2358867540984,79.1180567371074,201.9164562534));
#27974=CARTESIAN_POINT('Ctrl Pts',(78.5207761799292,79.4208792557371,201.942820956645));
#27975=CARTESIAN_POINT('Ctrl Pts',(78.6306947572285,79.5944745243928,201.957014557878));
#27976=CARTESIAN_POINT('Ctrl Pts',(78.7824296010498,79.9808002601524,201.987000948317));
#27977=CARTESIAN_POINT('Ctrl Pts',(78.8199584472721,80.1910568647587,202.002544578073));
#27978=CARTESIAN_POINT('Ctrl Pts',(78.8111368859214,80.6102990582761,202.032096322967));
#27979=CARTESIAN_POINT('Ctrl Pts',(78.7663473376232,80.8151555974517,202.04486045999));
#27980=CARTESIAN_POINT('Ctrl Pts',(78.6016170787386,81.1947886023995,202.072663062479));
#27981=CARTESIAN_POINT('Ctrl Pts',(78.4838674210283,81.3661604151088,202.08750195263));
#27982=CARTESIAN_POINT('Ctrl Pts',(78.184136943868,81.6604923331254,202.118129942819));
#27983=CARTESIAN_POINT('Ctrl Pts',(78.0027702393406,81.7783566227766,202.133630081357));
#27984=CARTESIAN_POINT('Ctrl Pts',(77.6143641095551,81.9317426641497,202.161838500422));
#27985=CARTESIAN_POINT('Ctrl Pts',(77.4127123815164,81.969692995123,202.174239265294));
#27986=CARTESIAN_POINT('Ctrl Pts',(77.0008164813083,81.967998794392,202.203096481991));
#27987=CARTESIAN_POINT('Ctrl Pts',(76.7945328665446,81.9264079908878,202.218383890842));
#27988=CARTESIAN_POINT('Ctrl Pts',(76.4061079448048,81.7650485970622,202.24887211865));
#27989=CARTESIAN_POINT('Ctrl Pts',(76.228246120193,81.6454598752063,202.263769792534));
#27990=CARTESIAN_POINT('Ctrl Pts',(75.936023256796,81.3503159801701,202.290269065912));
#27991=CARTESIAN_POINT('Ctrl Pts',(75.8218523556062,81.1800726257038,202.304047890935));
#27992=CARTESIAN_POINT('Ctrl Pts',(75.6603051897079,80.7986774888497,202.333854035404));
#27993=CARTESIAN_POINT('Ctrl Pts',(75.6172481277875,80.5900740663342,202.349375801221));
#27994=CARTESIAN_POINT('Ctrl Pts',(75.6145538929958,80.1698427195119,202.379196076377));
#27995=CARTESIAN_POINT('Ctrl Pts',(75.6542734625885,79.9624016441777,202.392269966595));
#27996=CARTESIAN_POINT('Ctrl Pts',(75.8099217931421,79.5779335637995,202.419837008763));
#27997=CARTESIAN_POINT('Ctrl Pts',(75.9230336172966,79.4040863928646,202.43455592085));
#27998=CARTESIAN_POINT('Ctrl Pts',(76.2143656873324,79.1029285681267,202.465084638613));
#27999=CARTESIAN_POINT('Ctrl Pts',(76.3921036130363,78.9806865815961,202.480613800882));
#28000=CARTESIAN_POINT('Ctrl Pts',(76.6694358785856,78.8625050380408,202.501191377896));
#28001=CARTESIAN_POINT('Ctrl Pts',(76.7527509576043,78.8348632894291,202.506977371544));
#28002=CARTESIAN_POINT('Ctrl Pts',(76.8377292359511,78.8141945740679,202.512499998088));
#28003=CARTESIAN_POINT('Ctrl Pts',(76.8377292359516,78.8141945740678,202.6));
#28004=CARTESIAN_POINT('Ctrl Pts',(76.6646070678815,78.856301955909,202.588749017992));
#28005=CARTESIAN_POINT('Ctrl Pts',(76.4995220554568,78.927069548299,202.57647890982));
#28006=CARTESIAN_POINT('Ctrl Pts',(76.1727024693801,79.1376303595131,202.54864000143));
#28007=CARTESIAN_POINT('Ctrl Pts',(76.0202253226858,79.2850865375819,202.533173635364));
#28008=CARTESIAN_POINT('Ctrl Pts',(75.785085469934,79.6245399372925,202.503680475096));
#28009=CARTESIAN_POINT('Ctrl Pts',(75.7023808492954,79.8116672127639,202.490559709967));
#28010=CARTESIAN_POINT('Ctrl Pts',(75.60907673497,80.2161288047186,202.463511044933));
#28011=CARTESIAN_POINT('Ctrl Pts',(75.6030216878962,80.4304323543675,202.448431750691));
#28012=CARTESIAN_POINT('Ctrl Pts',(75.6740690524535,80.8442431514089,202.41788847292));
#28013=CARTESIAN_POINT('Ctrl Pts',(75.7487034949919,81.0401163284464,202.40272449686));
#28014=CARTESIAN_POINT('Ctrl Pts',(75.9669404037729,81.3896371253457,202.374199769453));
#28015=CARTESIAN_POINT('Ctrl Pts',(76.107357250502,81.5406148905507,202.361878505874));
#28016=CARTESIAN_POINT('Ctrl Pts',(76.444720054825,81.7869127503183,202.33322198109));
#28017=CARTESIAN_POINT('Ctrl Pts',(76.6404150839586,81.8769616733207,202.317682039826));
#28018=CARTESIAN_POINT('Ctrl Pts',(77.0476648644173,81.9731814942715,202.287212006857));
#28019=CARTESIAN_POINT('Ctrl Pts',(77.2546353041046,81.9815200715456,202.272558262148));
#28020=CARTESIAN_POINT('Ctrl Pts',(77.6652092200424,81.9187758298425,202.2451146446));
#28021=CARTESIAN_POINT('Ctrl Pts',(77.8645728091164,81.8464785613806,202.231848865544));
#28022=CARTESIAN_POINT('Ctrl Pts',(78.2245532592939,81.6285998555793,202.201892517827));
#28023=CARTESIAN_POINT('Ctrl Pts',(78.3814638780194,81.4850000600263,202.186386486057));
#28024=CARTESIAN_POINT('Ctrl Pts',(78.6261457339997,81.1513913913891,202.156684335572));
#28025=CARTESIAN_POINT('Ctrl Pts',(78.7139194375733,80.9663568862993,202.143148093666));
#28026=CARTESIAN_POINT('Ctrl Pts',(78.8179992237349,80.5644096613865,202.116463267638));
#28027=CARTESIAN_POINT('Ctrl Pts',(78.829766885834,80.3503835666105,202.101502074866));
#28028=CARTESIAN_POINT('Ctrl Pts',(78.7697317797069,79.9343326915472,202.070989855529));
#28029=CARTESIAN_POINT('Ctrl Pts',(78.7000767279325,79.7360532648683,202.05574120217));
#28030=CARTESIAN_POINT('Ctrl Pts',(78.4909851176621,79.3811667102691,202.026993902738));
#28031=CARTESIAN_POINT('Ctrl Pts',(78.3550679719725,79.2270733216115,202.014640712796));
#28032=CARTESIAN_POINT('Ctrl Pts',(78.0245761176084,78.9718244017,201.986281472537));
#28033=CARTESIAN_POINT('Ctrl Pts',(77.8308069317692,78.8763664334322,201.970765398229));
#28034=CARTESIAN_POINT('Ctrl Pts',(77.4251468706189,78.7693327543938,201.940184904414));
#28035=CARTESIAN_POINT('Ctrl Pts',(77.2179313168644,78.755690162093,201.925405266856));
#28036=CARTESIAN_POINT('Ctrl Pts',(76.9544226574544,78.7892401951527,201.907654035774));
#28037=CARTESIAN_POINT('Ctrl Pts',(76.8956524436015,78.8001062880373,201.903764353083));
#28038=CARTESIAN_POINT('Ctrl Pts',(76.8377292359518,78.8141945740677,201.9));
#28039=CARTESIAN_POINT('Origin',(77.215862801455,80.368869783441,212.));
#28040=CARTESIAN_POINT('',(76.8377292359511,78.8141945740679,203.3));
#28041=CARTESIAN_POINT('',(76.8377292359512,78.8141945740679,203.212499998088));
#28042=CARTESIAN_POINT('',(76.8377292359511,78.8141945740678,212.));
#28043=CARTESIAN_POINT('Ctrl Pts',(76.8377292359511,78.8141945740679,202.512499998088));
#28044=CARTESIAN_POINT('Ctrl Pts',(76.9500920619865,78.7868652928247,202.51980231037));
#28045=CARTESIAN_POINT('Ctrl Pts',(77.0653056844449,78.7717391726939,202.527554292286));
#28046=CARTESIAN_POINT('Ctrl Pts',(77.3893336275295,78.7647665223466,202.550085249776));
#28047=CARTESIAN_POINT('Ctrl Pts',(77.5960944244831,78.8008631407702,202.56529340978));
#28048=CARTESIAN_POINT('Ctrl Pts',(77.9882175675707,78.95165226197,202.595823713416));
#28049=CARTESIAN_POINT('Ctrl Pts',(78.1692291048146,79.0664961932466,202.610844513016));
#28050=CARTESIAN_POINT('Ctrl Pts',(78.4690258570057,79.3536327069185,202.637709606131));
#28051=CARTESIAN_POINT('Ctrl Pts',(78.5875269392153,79.5205057199764,202.651029892044));
#28052=CARTESIAN_POINT('Ctrl Pts',(78.7589742726706,79.8965755449381,202.680629338512));
#28053=CARTESIAN_POINT('Ctrl Pts',(78.8076379840997,80.1033365357275,202.69611718347));
#28054=CARTESIAN_POINT('Ctrl Pts',(78.8221977655505,80.5244400183927,202.726203725202));
#28055=CARTESIAN_POINT('Ctrl Pts',(78.7877185822718,80.7345799163406,202.739676345269));
#28056=CARTESIAN_POINT('Ctrl Pts',(78.641334871577,81.1239004584044,202.766999066895));
#28057=CARTESIAN_POINT('Ctrl Pts',(78.5329669010044,81.3001267103364,202.781587561648));
#28058=CARTESIAN_POINT('Ctrl Pts',(78.2502851872322,81.6079556529771,202.811995925023));
#28059=CARTESIAN_POINT('Ctrl Pts',(78.0763213489491,81.7345190774253,202.827543614474));
#28060=CARTESIAN_POINT('Ctrl Pts',(77.6965039804361,81.9086498271757,202.856343525423));
#28061=CARTESIAN_POINT('Ctrl Pts',(77.4957458395885,81.9574553264438,202.868679877669));
#28062=CARTESIAN_POINT('Ctrl Pts',(77.0839964270015,81.9768602172663,202.89709427811));
#28063=CARTESIAN_POINT('Ctrl Pts',(76.876902972486,81.9462428206874,202.912213382904));
#28064=CARTESIAN_POINT('Ctrl Pts',(76.4813781696558,81.8060847737485,202.942763763888));
#28065=CARTESIAN_POINT('Ctrl Pts',(76.2973534315962,81.6960615643215,202.957896580053));
#28066=CARTESIAN_POINT('Ctrl Pts',(75.9900755620327,81.4169853029186,202.985119917269));
#28067=CARTESIAN_POINT('Ctrl Pts',(75.8672527319711,81.2533980005801,202.998070339886));
#28068=CARTESIAN_POINT('Ctrl Pts',(75.6861337459197,80.8826307577042,203.027460760865));
#28069=CARTESIAN_POINT('Ctrl Pts',(75.6320182500649,80.6778267302832,203.042903901538));
#28070=CARTESIAN_POINT('Ctrl Pts',(75.6057201100339,80.2560113946526,203.073243161843));
#28071=CARTESIAN_POINT('Ctrl Pts',(75.6349904960173,80.0431724977292,203.087186166083));
#28072=CARTESIAN_POINT('Ctrl Pts',(75.772297337779,79.6491760351658,203.11426558087));
#28073=CARTESIAN_POINT('Ctrl Pts',(75.8760123302209,79.4707613901058,203.12871885026));
#28074=CARTESIAN_POINT('Ctrl Pts',(76.1501523617184,79.1566841957607,203.158991299902));
#28075=CARTESIAN_POINT('Ctrl Pts',(76.3203551504402,79.0260304256433,203.174546568817));
#28076=CARTESIAN_POINT('Ctrl Pts',(76.6156282801234,78.8811637812547,203.197413972362));
#28077=CARTESIAN_POINT('Ctrl Pts',(76.7251381748456,78.8415793674466,203.20518285311));
#28078=CARTESIAN_POINT('Ctrl Pts',(76.8377292359512,78.8141945740678,203.212499998088));
#28079=CARTESIAN_POINT('Ctrl Pts',(76.8377292359511,78.8141945740679,203.3));
#28080=CARTESIAN_POINT('Ctrl Pts',(76.6372977216527,78.8629442310278,203.286974219498));
#28081=CARTESIAN_POINT('Ctrl Pts',(76.4480122774094,78.9500342613071,203.272605893883));
#28082=CARTESIAN_POINT('Ctrl Pts',(76.1108217964156,79.1930409508577,203.242586366163));
#28083=CARTESIAN_POINT('Ctrl Pts',(75.9668196527448,79.3473072665555,203.227224106349));
#28084=CARTESIAN_POINT('Ctrl Pts',(75.7494649935569,79.6973827808235,203.198134164226));
#28085=CARTESIAN_POINT('Ctrl Pts',(75.6762084806871,79.8885959629813,203.185560243896));
#28086=CARTESIAN_POINT('Ctrl Pts',(75.6034036952677,80.2975370860574,203.157840941478));
#28087=CARTESIAN_POINT('Ctrl Pts',(75.6081911415612,80.511934678872,203.142568139288));
#28088=CARTESIAN_POINT('Ctrl Pts',(75.6998893912881,80.9206962237656,203.112026737038));
#28089=CARTESIAN_POINT('Ctrl Pts',(75.7837462118058,81.1116738560253,203.097050689625));
#28090=CARTESIAN_POINT('Ctrl Pts',(76.0192541893987,81.4508407679873,203.068961919911));
#28091=CARTESIAN_POINT('Ctrl Pts',(76.1684804602313,81.595870075341,203.056468577965));
#28092=CARTESIAN_POINT('Ctrl Pts',(76.5188873796324,81.824638891677,203.027258663057));
#28093=CARTESIAN_POINT('Ctrl Pts',(76.7178923993662,81.9041376018337,203.011703401217));
#28094=CARTESIAN_POINT('Ctrl Pts',(77.1274173827322,81.9794214382293,202.981503382356));
#28095=CARTESIAN_POINT('Ctrl Pts',(77.3335325747862,81.9775639318118,202.967118520072));
#28096=CARTESIAN_POINT('Ctrl Pts',(77.7431344316525,81.8945236225489,202.940159024976));
#28097=CARTESIAN_POINT('Ctrl Pts',(77.9419643006599,81.8105649155683,202.925958811281));
#28098=CARTESIAN_POINT('Ctrl Pts',(78.2914932282357,81.5717502819813,202.895499590603));
#28099=CARTESIAN_POINT('Ctrl Pts',(78.4396099246003,81.420701942175,202.880082342266));
#28100=CARTESIAN_POINT('Ctrl Pts',(78.665531412132,81.0756999302961,202.850796012158));
#28101=CARTESIAN_POINT('Ctrl Pts',(78.7433412207922,80.8864863936483,202.837996197978));
#28102=CARTESIAN_POINT('Ctrl Pts',(78.8260886097391,80.4796673400736,202.810598583886));
#28103=CARTESIAN_POINT('Ctrl Pts',(78.8265534067992,80.2652446547458,202.795414513933));
#28104=CARTESIAN_POINT('Ctrl Pts',(78.7448180217156,79.8539070798602,202.76486228372));
#28105=CARTESIAN_POINT('Ctrl Pts',(78.6653915531734,79.6605044068468,202.749790766244));
#28106=CARTESIAN_POINT('Ctrl Pts',(78.438240109404,79.3162917588312,202.721488505881));
#28107=CARTESIAN_POINT('Ctrl Pts',(78.2933285442398,79.1683714342946,202.709117001913));
#28108=CARTESIAN_POINT('Ctrl Pts',(77.9492420811693,78.9310170139922,202.680173343095));
#28109=CARTESIAN_POINT('Ctrl Pts',(77.7517825479673,78.8463604418928,202.664620482353));
#28110=CARTESIAN_POINT('Ctrl Pts',(77.3432353358874,78.7608667615476,202.634279564757));
#28111=CARTESIAN_POINT('Ctrl Pts',(77.1366405681677,78.7577638908535,202.619759448272));
#28112=CARTESIAN_POINT('Ctrl Pts',(76.9023534571558,78.7995343618604,202.604221532181));
#28113=CARTESIAN_POINT('Ctrl Pts',(76.8699047618658,78.8063687296325,202.602091045111));
#28114=CARTESIAN_POINT('Ctrl Pts',(76.8377292359516,78.8141945740678,202.6));
#28115=CARTESIAN_POINT('Origin',(77.215862801455,80.368869783441,212.));
#28116=CARTESIAN_POINT('',(76.837729235951,78.8141945740679,204.));
#28117=CARTESIAN_POINT('',(76.8377292359514,78.8141945740678,203.912499998088));
#28118=CARTESIAN_POINT('',(76.8377292359511,78.8141945740678,212.));
#28119=CARTESIAN_POINT('Ctrl Pts',(76.8377292359512,78.8141945740678,203.212499998088));
#28120=CARTESIAN_POINT('Ctrl Pts',(76.9241273372014,78.7931805243927,203.218114897055));
#28121=CARTESIAN_POINT('Ctrl Pts',(77.012306563947,78.7793593757555,203.224001896763));
#28122=CARTESIAN_POINT('Ctrl Pts',(77.3077870837124,78.7581666254124,203.244243708424));
#28123=CARTESIAN_POINT('Ctrl Pts',(77.5150650290347,78.7835412677283,203.259268237987));
#28124=CARTESIAN_POINT('Ctrl Pts',(77.913576391502,78.9134437113486,203.289817347387));
#28125=CARTESIAN_POINT('Ctrl Pts',(78.1003640252084,79.018771336565,203.305047230497));
#28126=CARTESIAN_POINT('Ctrl Pts',(78.4147392583877,79.2900531834865,203.332607408692));
#28127=CARTESIAN_POINT('Ctrl Pts',(78.5417125300506,79.4505578745941,203.345284507738));
#28128=CARTESIAN_POINT('Ctrl Pts',(78.7319167218548,79.8162553533708,203.374472292603));
#28129=CARTESIAN_POINT('Ctrl Pts',(78.7911220914528,80.0190802911365,203.389862924639));
#28130=CARTESIAN_POINT('Ctrl Pts',(78.8283685512414,80.4390815528904,203.4202623244));
#28131=CARTESIAN_POINT('Ctrl Pts',(78.8048153931099,80.6521430613691,203.434623965844));
#28132=CARTESIAN_POINT('Ctrl Pts',(78.6785510432537,81.0486930086231,203.461249538411));
#28133=CARTESIAN_POINT('Ctrl Pts',(78.58006767538,81.2294021349393,203.475542404649));
#28134=CARTESIAN_POINT('Ctrl Pts',(78.3155969671828,81.5501669294063,203.50564158689));
#28135=CARTESIAN_POINT('Ctrl Pts',(78.1496908439536,81.6852500983994,203.521193256682));
#28136=CARTESIAN_POINT('Ctrl Pts',(77.7792024180381,81.8806537051101,203.550572212483));
#28137=CARTESIAN_POINT('Ctrl Pts',(77.5791959821053,81.9407545056932,203.563182834373));
#28138=CARTESIAN_POINT('Ctrl Pts',(77.1678707790729,81.9814097036313,203.591131884754));
#28139=CARTESIAN_POINT('Ctrl Pts',(76.9605411325661,81.9617818432542,203.60604221372));
#28140=CARTESIAN_POINT('Ctrl Pts',(76.5570052405901,81.8426078743946,203.636722964176));
#28141=CARTESIAN_POINT('Ctrl Pts',(76.3655752667733,81.7411103402857,203.652199172683));
#28142=CARTESIAN_POINT('Ctrl Pts',(76.042919470818,81.4758765817549,203.680214788941));
#28143=CARTESIAN_POINT('Ctrl Pts',(75.9120212040928,81.3182231903672,203.692705925547));
#28144=CARTESIAN_POINT('Ctrl Pts',(75.7134116942629,80.9572917520173,203.721700877182));
#28145=CARTESIAN_POINT('Ctrl Pts',(75.6495313326676,80.75641830372,203.737033806571));
#28146=CARTESIAN_POINT('Ctrl Pts',(75.6021520058948,80.3381721085283,203.76748347411));
#28147=CARTESIAN_POINT('Ctrl Pts',(75.6204264800724,80.1246547157139,203.78229649554));
#28148=CARTESIAN_POINT('Ctrl Pts',(75.7392370785646,79.7172975776863,203.809110768139));
#28149=CARTESIAN_POINT('Ctrl Pts',(75.8385447395526,79.5273909602021,203.823891447406));
#28150=CARTESIAN_POINT('Ctrl Pts',(76.1035016204051,79.1999979744398,203.854349997429));
#28151=CARTESIAN_POINT('Ctrl Pts',(76.2653990345763,79.0649378230296,203.869689078905));
#28152=CARTESIAN_POINT('Ctrl Pts',(76.5714943646726,78.8976877949465,203.894254263654));
#28153=CARTESIAN_POINT('Ctrl Pts',(76.7022797579508,78.8471390718981,203.90369731466));
#28154=CARTESIAN_POINT('Ctrl Pts',(76.8377292359517,78.8141945740677,203.912499998088));
#28155=CARTESIAN_POINT('Ctrl Pts',(76.837729235951,78.8141945740679,204.));
#28156=CARTESIAN_POINT('Ctrl Pts',(76.8164855339289,78.8193615418961,203.998619399746));
#28157=CARTESIAN_POINT('Ctrl Pts',(76.7953336269056,78.8249673612387,203.997221545057));
#28158=CARTESIAN_POINT('Ctrl Pts',(76.5702076437519,78.8896092732629,203.982093149827));
#28159=CARTESIAN_POINT('Ctrl Pts',(76.379877358006,78.988231115077,203.967089096228));
#28160=CARTESIAN_POINT('Ctrl Pts',(76.052182681302,79.2512379244776,203.93656340598));
#28161=CARTESIAN_POINT('Ctrl Pts',(75.9168985765468,79.4118106224138,203.92134343455));
#28162=CARTESIAN_POINT('Ctrl Pts',(75.7173468648551,79.7721845900864,203.892673943122));
#28163=CARTESIAN_POINT('Ctrl Pts',(75.6535940004212,79.9677531423396,203.880341579362));
#28164=CARTESIAN_POINT('Ctrl Pts',(75.6017095244076,80.3821222569537,203.851877185503));
#28165=CARTESIAN_POINT('Ctrl Pts',(75.617910585001,80.5973130085841,203.836351500336));
#28166=CARTESIAN_POINT('Ctrl Pts',(75.7316246771356,81.0007568706779,203.805807470381));
#28167=CARTESIAN_POINT('Ctrl Pts',(75.8249951750216,81.1860397767841,203.79107095462));
#28168=CARTESIAN_POINT('Ctrl Pts',(76.0788889363189,81.5138488439366,203.763470064755));
#28169=CARTESIAN_POINT('Ctrl Pts',(76.2379921095794,81.6524110555826,203.750445306723));
#28170=CARTESIAN_POINT('Ctrl Pts',(76.6023298567526,81.86155586569,203.720662903977));
#28171=CARTESIAN_POINT('Ctrl Pts',(76.8043330498887,81.929373209693,203.705137331507));
#28172=CARTESIAN_POINT('Ctrl Pts',(77.2153498303632,81.9817368008845,203.675302826279));
#28173=CARTESIAN_POINT('Ctrl Pts',(77.4199800269579,81.9687392875352,203.661453567262));
#28174=CARTESIAN_POINT('Ctrl Pts',(77.8221215248086,81.8647030127121,203.635005444164));
#28175=CARTESIAN_POINT('Ctrl Pts',(78.0149588024898,81.7711753785389,203.620125656083));
#28176=CARTESIAN_POINT('Ctrl Pts',(78.3499058242012,81.5166596610425,203.589644980771));
#28177=CARTESIAN_POINT('Ctrl Pts',(78.4896859687075,81.359255298631,203.574347400866));
#28178=CARTESIAN_POINT('Ctrl Pts',(78.6983654995234,81.0041209070582,203.54546029511));
#28179=CARTESIAN_POINT('Ctrl Pts',(78.7670003086117,80.8108199384722,203.533042856392));
#28180=CARTESIAN_POINT('Ctrl Pts',(78.8298836226726,80.397973906022,203.504875913675));
#28181=CARTESIAN_POINT('Ctrl Pts',(78.8192659813997,80.1818536772977,203.489380591157));
#28182=CARTESIAN_POINT('Ctrl Pts',(78.71562951968,79.7746029993714,203.458740508447));
#28183=CARTESIAN_POINT('Ctrl Pts',(78.6267107702664,79.5865698158039,203.443885847968));
#28184=CARTESIAN_POINT('Ctrl Pts',(78.3815021773898,79.2533512277332,203.416051356147));
#28185=CARTESIAN_POINT('Ctrl Pts',(78.2271316518134,79.1117122007809,203.403323256942));
#28186=CARTESIAN_POINT('Ctrl Pts',(77.8693760757632,78.8931687495223,203.373808755235));
#28187=CARTESIAN_POINT('Ctrl Pts',(77.6687173886042,78.8197782963812,203.35826300697));
#28188=CARTESIAN_POINT('Ctrl Pts',(77.258361291222,78.7565235724923,203.32825144718));
#28189=CARTESIAN_POINT('Ctrl Pts',(77.0529632663945,78.7641962158736,203.314035988574));
#28190=CARTESIAN_POINT('Ctrl Pts',(76.8488878959581,78.8115122881281,203.300725837822));
#28191=CARTESIAN_POINT('Ctrl Pts',(76.843304322095,78.8128385820325,203.300362317516));
#28192=CARTESIAN_POINT('Ctrl Pts',(76.8377292359511,78.8141945740679,203.3));
#28193=CARTESIAN_POINT('Origin',(77.215862801455,80.368869783441,212.));
#28194=CARTESIAN_POINT('',(76.8377292359508,78.8141945740679,204.7));
#28195=CARTESIAN_POINT('',(76.8377292359514,78.8141945740678,204.612499998088));
#28196=CARTESIAN_POINT('',(76.8377292359511,78.8141945740678,212.));
#28197=CARTESIAN_POINT('Ctrl Pts',(76.8377292359517,78.8141945740677,203.912499998088));
#28198=CARTESIAN_POINT('Ctrl Pts',(76.8988718220249,78.7993232595085,203.916473574341));
#28199=CARTESIAN_POINT('Ctrl Pts',(76.9609484409753,78.7880445652141,203.920586164267));
#28200=CARTESIAN_POINT('Ctrl Pts',(77.2345219185842,78.7549405019645,203.939050825753));
#28201=CARTESIAN_POINT('Ctrl Pts',(77.4483288436784,78.7716722576286,203.954355028478));
#28202=CARTESIAN_POINT('Ctrl Pts',(77.851172785091,78.8859699802009,203.984887388585));
#28203=CARTESIAN_POINT('Ctrl Pts',(78.0370246036382,78.9802253934054,203.999824789487));
#28204=CARTESIAN_POINT('Ctrl Pts',(78.3628087403947,79.2343114574565,204.027830765998));
#28205=CARTESIAN_POINT('Ctrl Pts',(78.49957164793,79.3917273975043,204.040390105629));
#28206=CARTESIAN_POINT('Ctrl Pts',(78.7083973684543,79.7546288016049,204.069700683849));
#28207=CARTESIAN_POINT('Ctrl Pts',(78.7765593331449,79.9575757023486,204.085254302958));
#28208=CARTESIAN_POINT('Ctrl Pts',(78.8288169372792,80.3702798779705,204.115395378047));
#28209=CARTESIAN_POINT('Ctrl Pts',(78.8155049889549,80.5757823535477,204.129726051018));
#28210=CARTESIAN_POINT('Ctrl Pts',(78.7097250467114,80.9806973275376,204.15659184709));
#28211=CARTESIAN_POINT('Ctrl Pts',(78.6143813798786,81.1752118164232,204.171004160665));
#28212=CARTESIAN_POINT('Ctrl Pts',(78.355720693294,81.511032958448,204.201554986642));
#28213=CARTESIAN_POINT('Ctrl Pts',(78.1966810946415,81.6502032825951,204.216950284698));
#28214=CARTESIAN_POINT('Ctrl Pts',(77.8396015994553,81.856189009366,204.246154823755));
#28215=CARTESIAN_POINT('Ctrl Pts',(77.6462404194208,81.923192277403,204.258851443234));
#28216=CARTESIAN_POINT('Ctrl Pts',(77.2353161315612,81.9827870629292,204.286384147099));
#28217=CARTESIAN_POINT('Ctrl Pts',(77.0211989834806,81.9711101397455,204.301606425426));
#28218=CARTESIAN_POINT('Ctrl Pts',(76.615335803055,81.8662585490563,204.332156396177));
#28219=CARTESIAN_POINT('Ctrl Pts',(76.4269128279573,81.7761329740433,204.347189045765));
#28220=CARTESIAN_POINT('Ctrl Pts',(76.0958707106108,81.5298631867101,204.375402703916));
#28221=CARTESIAN_POINT('Ctrl Pts',(75.9561209801514,81.376511614043,204.387816171576));
#28222=CARTESIAN_POINT('Ctrl Pts',(75.7386702935091,81.019310546269,204.416871505808));
#28223=CARTESIAN_POINT('Ctrl Pts',(75.6654390627978,80.8175766914384,204.432426536183));
#28224=CARTESIAN_POINT('Ctrl Pts',(75.6032591828435,80.4052628385412,204.462710943586));
#28225=CARTESIAN_POINT('Ctrl Pts',(75.6118021416659,80.1990274982907,204.477175723138));
#28226=CARTESIAN_POINT('Ctrl Pts',(75.7079797728761,79.7931454698215,204.504275509328));
#28227=CARTESIAN_POINT('Ctrl Pts',(75.7977057640665,79.5981176371529,204.518176447608));
#28228=CARTESIAN_POINT('Ctrl Pts',(76.0466229463546,79.256702584626,204.548495027017));
#28229=CARTESIAN_POINT('Ctrl Pts',(76.2024148198878,79.1130975564851,204.563942316811));
#28230=CARTESIAN_POINT('Ctrl Pts',(76.5230643351593,78.9171242773603,204.59072132588));
#28231=CARTESIAN_POINT('Ctrl Pts',(76.6769744816766,78.8532939100829,204.602052758037));
#28232=CARTESIAN_POINT('Ctrl Pts',(76.8377292359517,78.8141945740677,204.612499998088));
#28233=CARTESIAN_POINT('Ctrl Pts',(76.8377292359504,78.814194574068,204.7));
#28234=CARTESIAN_POINT('Ctrl Pts',(76.7895023846101,78.8259244782567,204.696865800361));
#28235=CARTESIAN_POINT('Ctrl Pts',(76.7417728761323,78.839910017265,204.693644261852));
#28236=CARTESIAN_POINT('Ctrl Pts',(76.4938954972622,78.9253081860543,204.676270834625));
#28237=CARTESIAN_POINT('Ctrl Pts',(76.3089114608851,79.0337642943317,204.661053605709));
#28238=CARTESIAN_POINT('Ctrl Pts',(75.9961373947811,79.3128929183864,204.630503141403));
#28239=CARTESIAN_POINT('Ctrl Pts',(75.869912812526,79.4793409245744,204.615465173399));
#28240=CARTESIAN_POINT('Ctrl Pts',(75.6884760444571,79.8498753363947,204.587239536817));
#28241=CARTESIAN_POINT('Ctrl Pts',(75.634506484563,80.0501519397626,204.574832463734));
#28242=CARTESIAN_POINT('Ctrl Pts',(75.6048059548743,80.4672542826168,204.545792129521));
#28243=CARTESIAN_POINT('Ctrl Pts',(75.6321123575831,80.6801553782358,204.530237294496));
#28244=CARTESIAN_POINT('Ctrl Pts',(75.765719886486,81.0752064958853,204.499945082958));
#28245=CARTESIAN_POINT('Ctrl Pts',(75.8677994169808,81.2546423771457,204.485472755538));
#28246=CARTESIAN_POINT('Ctrl Pts',(76.1391774391111,81.5713152242223,204.458359578796));
#28247=CARTESIAN_POINT('Ctrl Pts',(76.3081802069298,81.703521786783,204.444486029876));
#28248=CARTESIAN_POINT('Ctrl Pts',(76.6857425560261,81.8930165113386,204.41418109223));
#28249=CARTESIAN_POINT('Ctrl Pts',(76.8900327571334,81.9493406730169,204.398731114972));
#28250=CARTESIAN_POINT('Ctrl Pts',(77.3016575938514,81.9793913559084,204.369311511891));
#28251=CARTESIAN_POINT('Ctrl Pts',(77.5048308707005,81.9555633877178,204.356314921111));
#28252=CARTESIAN_POINT('Ctrl Pts',(77.9006129346417,81.8304487340569,204.329140925675));
#28253=CARTESIAN_POINT('Ctrl Pts',(78.0882869780496,81.7267830290852,204.314023013219));
#28254=CARTESIAN_POINT('Ctrl Pts',(78.408484830022,81.455462088244,204.283474112372));
#28255=CARTESIAN_POINT('Ctrl Pts',(78.5391868263776,81.2918354512038,204.26834204869));
#28256=CARTESIAN_POINT('Ctrl Pts',(78.7295346840857,80.9262629150247,204.23989624657));
#28257=CARTESIAN_POINT('Ctrl Pts',(78.7883371621984,80.7283325701793,204.227566227471));
#28258=CARTESIAN_POINT('Ctrl Pts',(78.8290107934515,80.3125269232905,204.198806861185));
#28259=CARTESIAN_POINT('Ctrl Pts',(78.8071692961944,80.0984247812819,204.183261105522));
#28260=CARTESIAN_POINT('Ctrl Pts',(78.6833257917591,79.6991052315307,204.152834730954));
#28261=CARTESIAN_POINT('Ctrl Pts',(78.5855074054855,79.5167285662415,204.138227476604));
#28262=CARTESIAN_POINT('Ctrl Pts',(78.3227723413209,79.1945090391943,204.110870252639));
#28263=CARTESIAN_POINT('Ctrl Pts',(78.1587258780098,79.0591300213629,204.09745853139));
#28264=CARTESIAN_POINT('Ctrl Pts',(77.7876934999827,78.8597972340702,204.067408833216));
#28265=CARTESIAN_POINT('Ctrl Pts',(77.5844613521762,78.7977480600917,204.051915521329));
#28266=CARTESIAN_POINT('Ctrl Pts',(77.1948987284957,78.7587945493212,204.023857202725));
#28267=CARTESIAN_POINT('Ctrl Pts',(77.0132492514773,78.7715039793455,204.011406814961));
#28268=CARTESIAN_POINT('Ctrl Pts',(76.837729235951,78.8141945740679,204.));
#28269=CARTESIAN_POINT('Origin',(77.215862801455,80.368869783441,212.));
#28270=CARTESIAN_POINT('',(76.8377292359511,78.8141945740679,205.4));
#28271=CARTESIAN_POINT('',(76.8377292359511,78.8141945740679,205.312499998088));
#28272=CARTESIAN_POINT('',(76.8377292359511,78.8141945740678,212.));
#28273=CARTESIAN_POINT('Ctrl Pts',(76.8377292359517,78.8141945740677,204.612499998088));
#28274=CARTESIAN_POINT('Ctrl Pts',(76.87347087857,78.8055013662011,204.614822800434));
#28275=CARTESIAN_POINT('Ctrl Pts',(76.9095453758351,78.798032605701,204.617193997504));
#28276=CARTESIAN_POINT('Ctrl Pts',(77.1552066426569,78.7559788113551,204.633522013413));
#28277=CARTESIAN_POINT('Ctrl Pts',(77.3695205837571,78.7621829690208,204.648645861751));
#28278=CARTESIAN_POINT('Ctrl Pts',(77.7783972624879,78.8567279410647,204.67919540006));
#28279=CARTESIAN_POINT('Ctrl Pts',(77.9694989853232,78.9423100573504,204.694322347149));
#28280=CARTESIAN_POINT('Ctrl Pts',(78.3061629355851,79.1801080401349,204.722755708176));
#28281=CARTESIAN_POINT('Ctrl Pts',(78.4491193968819,79.3291646858567,204.735088043748));
#28282=CARTESIAN_POINT('Ctrl Pts',(78.6757029845035,79.6801941721309,204.763863498823));
#28283=CARTESIAN_POINT('Ctrl Pts',(78.7543279674699,79.8804964119921,204.779410046368));
#28284=CARTESIAN_POINT('Ctrl Pts',(78.8271145261591,80.2921341074044,204.809829328457));
#28285=CARTESIAN_POINT('Ctrl Pts',(78.8236929481159,80.4990300614199,204.82442916817));
#28286=CARTESIAN_POINT('Ctrl Pts',(78.7377174705474,80.9058713827151,204.851772731434));
#28287=CARTESIAN_POINT('Ctrl Pts',(78.6538446117614,81.1014397604285,204.86520838787));
#28288=CARTESIAN_POINT('Ctrl Pts',(78.4152265811471,81.4485934937248,204.895272703575));
#28289=CARTESIAN_POINT('Ctrl Pts',(78.2629901939392,81.5967945814601,204.910763877175));
#28290=CARTESIAN_POINT('Ctrl Pts',(77.9161651020494,81.8217182132772,204.940381086406));
#28291=CARTESIAN_POINT('Ctrl Pts',(77.7265052478057,81.8986978372163,204.953737074714));
#28292=CARTESIAN_POINT('Ctrl Pts',(77.3193282330171,81.9795770677055,204.980571196726));
#28293=CARTESIAN_POINT('Ctrl Pts',(77.1049626836357,81.979067594133,204.995581906058));
#28294=CARTESIAN_POINT('Ctrl Pts',(76.6932320133264,81.8953353051922,205.026109475268));
#28295=CARTESIAN_POINT('Ctrl Pts',(76.4994587495614,81.8145610697187,205.041324794478));
#28296=CARTESIAN_POINT('Ctrl Pts',(76.157008732524,81.5855974798968,205.069981917019));
#28297=CARTESIAN_POINT('Ctrl Pts',(76.0107423572109,81.4409137873655,205.082311936756));
#28298=CARTESIAN_POINT('Ctrl Pts',(75.7748581957499,81.0963025631212,205.110792924539));
#28299=CARTESIAN_POINT('Ctrl Pts',(75.6907226947701,80.8976152834975,205.126320011226));
#28300=CARTESIAN_POINT('Ctrl Pts',(75.6070466851493,80.4869502960989,205.156858029989));
#28301=CARTESIAN_POINT('Ctrl Pts',(75.6051851602486,80.2795082605422,205.171587602031));
#28302=CARTESIAN_POINT('Ctrl Pts',(75.6807397717952,79.8717584247721,205.199175113662));
#28303=CARTESIAN_POINT('Ctrl Pts',(75.7587530067581,79.6756333159173,205.212219109163));
#28304=CARTESIAN_POINT('Ctrl Pts',(75.9869140471254,79.3228268384665,205.242016509498));
#28305=CARTESIAN_POINT('Ctrl Pts',(76.1354151060354,79.1700590426472,205.257540603753));
#28306=CARTESIAN_POINT('Ctrl Pts',(76.4697255012955,78.9401624955558,205.286748139996));
#28307=CARTESIAN_POINT('Ctrl Pts',(76.648829935328,78.8601393255087,205.300223680986));
#28308=CARTESIAN_POINT('Ctrl Pts',(76.8377292359511,78.8141945740679,205.312499998088));
#28309=CARTESIAN_POINT('Ctrl Pts',(76.837729235951,78.8141945740679,205.4));
#28310=CARTESIAN_POINT('Ctrl Pts',(76.7551212011898,78.8342867904583,205.394631412469));
#28311=CARTESIAN_POINT('Ctrl Pts',(76.6740740682798,78.8609712158328,205.389013236702));
#28312=CARTESIAN_POINT('Ctrl Pts',(76.4047721719173,78.9742784392342,205.369104620904));
#28313=CARTESIAN_POINT('Ctrl Pts',(76.2315578549372,79.0906407584965,205.354110083167));
#28314=CARTESIAN_POINT('Ctrl Pts',(75.9350654447631,79.3867132329826,205.323565240702));
#28315=CARTESIAN_POINT('Ctrl Pts',(75.8161553456459,79.5651720045722,205.308308321444));
#28316=CARTESIAN_POINT('Ctrl Pts',(75.6585440861613,79.9494216629153,205.280648746899));
#28317=CARTESIAN_POINT('Ctrl Pts',(75.6179490665698,80.1500757283593,205.268038083199));
#28318=CARTESIAN_POINT('Ctrl Pts',(75.6138721890207,80.5621666080175,205.238911253169));
#28319=CARTESIAN_POINT('Ctrl Pts',(75.6528250702192,80.7696710992104,205.223538073735));
#28320=CARTESIAN_POINT('Ctrl Pts',(75.8095424391573,81.1609318663869,205.193116168863));
#28321=CARTESIAN_POINT('Ctrl Pts',(75.9269208027371,81.340274475958,205.178611880733));
#28322=CARTESIAN_POINT('Ctrl Pts',(76.2187671975469,81.6366838658313,205.152113006099));
#28323=CARTESIAN_POINT('Ctrl Pts',(76.3881892768247,81.7532332382239,205.137868216388));
#28324=CARTESIAN_POINT('Ctrl Pts',(76.7687972806784,81.9196559783247,205.107823171834));
#28325=CARTESIAN_POINT('Ctrl Pts',(76.9776681826639,81.9651407600593,205.092274884239));
#28326=CARTESIAN_POINT('Ctrl Pts',(77.3966940428623,81.9720875330056,205.062811061138));
#28327=CARTESIAN_POINT('Ctrl Pts',(77.6026659915845,81.9351962846408,205.050129378388));
#28328=CARTESIAN_POINT('Ctrl Pts',(77.988098075007,81.7852653846243,205.022251782484));
#28329=CARTESIAN_POINT('Ctrl Pts',(78.1639919457963,81.6740684619583,205.007375993244));
#28330=CARTESIAN_POINT('Ctrl Pts',(78.4640202909783,81.3909710588773,204.977297944441));
#28331=CARTESIAN_POINT('Ctrl Pts',(78.5853362915726,81.2216066863523,204.962372029918));
#28332=CARTESIAN_POINT('Ctrl Pts',(78.7570757738794,80.8457585555339,204.934390309712));
#28333=CARTESIAN_POINT('Ctrl Pts',(78.8057378661131,80.6428520706424,204.921809701669));
#28334=CARTESIAN_POINT('Ctrl Pts',(78.8233675643026,80.2244589851985,204.892469904537));
#28335=CARTESIAN_POINT('Ctrl Pts',(78.7901213237259,80.0130303360736,204.876917034798));
#28336=CARTESIAN_POINT('Ctrl Pts',(78.6459586495334,79.622929673399,204.846793675241));
#28337=CARTESIAN_POINT('Ctrl Pts',(78.5393029184471,79.446832765854,204.832479057667));
#28338=CARTESIAN_POINT('Ctrl Pts',(78.2600541470652,79.1381441568787,204.805795938984));
#28339=CARTESIAN_POINT('Ctrl Pts',(78.0877588221643,79.0105972118158,204.791497598391));
#28340=CARTESIAN_POINT('Ctrl Pts',(77.7059670624353,78.8314620415953,204.761109094792));
#28341=CARTESIAN_POINT('Ctrl Pts',(77.5008174194325,78.7805899862057,204.745710755011));
#28342=CARTESIAN_POINT('Ctrl Pts',(77.1387798153871,78.7634125216628,204.720024948583));
#28343=CARTESIAN_POINT('Ctrl Pts',(76.9859553886663,78.778142488533,204.709633022714));
#28344=CARTESIAN_POINT('Ctrl Pts',(76.8377292359504,78.814194574068,204.7));
#28345=CARTESIAN_POINT('Origin',(77.215862801455,80.368869783441,212.));
#28346=CARTESIAN_POINT('',(76.8377292359511,78.8141945740678,206.1));
#28347=CARTESIAN_POINT('',(76.8377292359511,78.8141945740678,206.012499998088));
#28348=CARTESIAN_POINT('',(76.8377292359511,78.8141945740678,212.));
#28349=CARTESIAN_POINT('Ctrl Pts',(76.8377292359512,78.8141945740679,205.312499998088));
#28350=CARTESIAN_POINT('Ctrl Pts',(76.8460262768778,78.8121765386288,205.313039211866));
#28351=CARTESIAN_POINT('Ctrl Pts',(76.8543419151689,78.8102243289544,205.313581076532));
#28352=CARTESIAN_POINT('Ctrl Pts',(77.0697299280818,78.761476620757,205.327653480417));
#28353=CARTESIAN_POINT('Ctrl Pts',(77.2839912443304,78.7563019461671,205.342540361718));
#28354=CARTESIAN_POINT('Ctrl Pts',(77.6982836699973,78.8291512923048,205.373024072114));
#28355=CARTESIAN_POINT('Ctrl Pts',(77.8946055301384,78.905044242438,205.388317655467));
#28356=CARTESIAN_POINT('Ctrl Pts',(78.2427681657401,79.1251520129856,205.417192960697));
#28357=CARTESIAN_POINT('Ctrl Pts',(78.3923340039078,79.2655685193145,205.429603623653));
#28358=CARTESIAN_POINT('Ctrl Pts',(78.6373109624049,79.6037671547505,205.457786965554));
#28359=CARTESIAN_POINT('Ctrl Pts',(78.7268457821231,79.8007200571218,205.473284214301));
#28360=CARTESIAN_POINT('Ctrl Pts',(78.8212444038845,80.2101508078975,205.503919565077));
#28361=CARTESIAN_POINT('Ctrl Pts',(78.8283330455804,80.4179993675096,205.518768016861));
#28362=CARTESIAN_POINT('Ctrl Pts',(78.7630008966621,80.8265711687446,205.546589925751));
#28363=CARTESIAN_POINT('Ctrl Pts',(78.6906234423817,81.0232560577664,205.559332073145));
#28364=CARTESIAN_POINT('Ctrl Pts',(78.4726526838346,81.3814108215029,205.588861295697));
#28365=CARTESIAN_POINT('Ctrl Pts',(78.3279091400948,81.5385286778803,205.604406232331));
#28366=CARTESIAN_POINT('Ctrl Pts',(77.9921441869454,81.7826739453617,205.634407900906));
#28367=CARTESIAN_POINT('Ctrl Pts',(77.8060708467818,81.8699216507472,205.648614750934));
#28368=CARTESIAN_POINT('Ctrl Pts',(77.4029701473195,81.9719846302046,205.675014110391));
#28369=CARTESIAN_POINT('Ctrl Pts',(77.1889124798798,81.9826756615117,205.689633534107));
#28370=CARTESIAN_POINT('Ctrl Pts',(76.7722099218598,81.9202722643828,205.720071734931));
#28371=CARTESIAN_POINT('Ctrl Pts',(76.5735641031912,81.8491197064306,205.735430751895));
#28372=CARTESIAN_POINT('Ctrl Pts',(76.2199957127401,81.6375193900391,205.764509909028));
#28373=CARTESIAN_POINT('Ctrl Pts',(76.0672719147115,81.5010992773044,205.777073575518));
#28374=CARTESIAN_POINT('Ctrl Pts',(75.8152137785069,81.170926829644,205.804810280769));
#28375=CARTESIAN_POINT('Ctrl Pts',(75.7212557212402,80.978153041104,205.820087658874));
#28376=CARTESIAN_POINT('Ctrl Pts',(75.6155250598987,80.5728204198378,205.850627933799));
#28377=CARTESIAN_POINT('Ctrl Pts',(75.6025781577021,80.3646728092727,205.865598527017));
#28378=CARTESIAN_POINT('Ctrl Pts',(75.6565391648345,79.955266773706,205.893675497214));
#28379=CARTESIAN_POINT('Ctrl Pts',(75.7227718583759,79.7579332428505,205.906177616559));
#28380=CARTESIAN_POINT('Ctrl Pts',(75.9294921770812,79.3940484602969,205.935401965953));
#28381=CARTESIAN_POINT('Ctrl Pts',(76.0699577027409,79.23224710885,205.95095708058));
#28382=CARTESIAN_POINT('Ctrl Pts',(76.399458871065,78.977764839473,205.9811488438));
#28383=CARTESIAN_POINT('Ctrl Pts',(76.5835011456803,78.8850062283669,205.99552604142));
#28384=CARTESIAN_POINT('Ctrl Pts',(76.7992031104156,78.8239456967837,206.009977069679));
#28385=CARTESIAN_POINT('Ctrl Pts',(76.8184288597615,78.8188888793608,206.011245692024));
#28386=CARTESIAN_POINT('Ctrl Pts',(76.837729235951,78.8141945740679,206.012499998088));
#28387=CARTESIAN_POINT('Ctrl Pts',(76.8377292359512,78.8141945740678,206.1));
#28388=CARTESIAN_POINT('Ctrl Pts',(76.7295564051995,78.84050474994,206.092969990001));
#28389=CARTESIAN_POINT('Ctrl Pts',(76.6242071338796,78.8780811547185,206.085521653149));
#28390=CARTESIAN_POINT('Ctrl Pts',(76.3360805833358,79.0164076254402,206.063360472326));
#28391=CARTESIAN_POINT('Ctrl Pts',(76.168093156805,79.1419510224239,206.048179351679));
#28392=CARTESIAN_POINT('Ctrl Pts',(75.886508064799,79.4535233937972,206.0176403473));
#28393=CARTESIAN_POINT('Ctrl Pts',(75.7769098452468,79.6377726232886,206.002583013583));
#28394=CARTESIAN_POINT('Ctrl Pts',(75.639207908886,80.0293590514828,205.975604104429));
#28395=CARTESIAN_POINT('Ctrl Pts',(75.6088938918627,80.231713904417,205.9624099746));
#28396=CARTESIAN_POINT('Ctrl Pts',(75.6258182785655,80.6444400980455,205.932876224462));
#28397=CARTESIAN_POINT('Ctrl Pts',(75.6757309294006,80.8507143613043,205.917401342142));
#28398=CARTESIAN_POINT('Ctrl Pts',(75.8530109775707,81.2333860441182,205.887233633762));
#28399=CARTESIAN_POINT('Ctrl Pts',(75.9790801299804,81.4057287529166,205.873620103953));
#28400=CARTESIAN_POINT('Ctrl Pts',(76.2860429984549,81.6869793327039,205.846374231918));
#28401=CARTESIAN_POINT('Ctrl Pts',(76.4622559443836,81.795058439425,205.831827904456));
#28402=CARTESIAN_POINT('Ctrl Pts',(76.8532605300127,81.9417045723369,205.801460810072));
#28403=CARTESIAN_POINT('Ctrl Pts',(77.0654675101779,81.9759456732983,205.785909593641));
#28404=CARTESIAN_POINT('Ctrl Pts',(77.4830873312372,81.9596700127071,205.757020256091));
#28405=CARTESIAN_POINT('Ctrl Pts',(77.6845014352316,81.9123823242378,205.744664500929));
#28406=CARTESIAN_POINT('Ctrl Pts',(78.0606130127198,81.7434070248921,205.716319616828));
#28407=CARTESIAN_POINT('Ctrl Pts',(78.2313468732561,81.6225539237121,205.701229796181));
#28408=CARTESIAN_POINT('Ctrl Pts',(78.5206962074919,81.3188536149637,205.670677640206));
#28409=CARTESIAN_POINT('Ctrl Pts',(78.6351165714267,81.1375178583068,205.655512666239));
#28410=CARTESIAN_POINT('Ctrl Pts',(78.7830619342441,80.749652677949,205.628180855822));
#28411=CARTESIAN_POINT('Ctrl Pts',(78.8186672663754,80.5482023002402,205.615326470681));
#28412=CARTESIAN_POINT('Ctrl Pts',(78.8126137889458,80.1357667896468,205.58600065032));
#28413=CARTESIAN_POINT('Ctrl Pts',(78.7683677270193,79.9287852247619,205.570573305253));
#28414=CARTESIAN_POINT('Ctrl Pts',(78.6010919413994,79.5402018279054,205.540159145476));
#28415=CARTESIAN_POINT('Ctrl Pts',(78.4783753241339,79.3631142207569,205.526058225016));
#28416=CARTESIAN_POINT('Ctrl Pts',(78.1772529375327,79.0736830296676,205.49905332579));
#28417=CARTESIAN_POINT('Ctrl Pts',(78.0041426461427,78.9616202196116,205.484642434675));
#28418=CARTESIAN_POINT('Ctrl Pts',(77.6178428989278,78.8057077498253,205.45441458712));
#28419=CARTESIAN_POINT('Ctrl Pts',(77.407112893485,78.7662143562072,205.438859041677));
#28420=CARTESIAN_POINT('Ctrl Pts',(77.0741725852005,78.7705959032636,205.415651318138));
#28421=CARTESIAN_POINT('Ctrl Pts',(76.9544243197534,78.7858115858727,205.407583860016));
#28422=CARTESIAN_POINT('Ctrl Pts',(76.837729235951,78.8141945740679,205.4));
#28423=CARTESIAN_POINT('Origin',(77.215862801455,80.368869783441,212.));
#28424=CARTESIAN_POINT('',(76.8377292359514,78.8141945740678,206.8));
#28425=CARTESIAN_POINT('',(76.8377292359507,78.8141945740679,206.712499998088));
#28426=CARTESIAN_POINT('',(76.8377292359511,78.8141945740678,212.));
#28427=CARTESIAN_POINT('Ctrl Pts',(76.837729235951,78.8141945740679,206.012499998088));
#28428=CARTESIAN_POINT('Ctrl Pts',(77.0257911158799,78.7684535030299,206.024721892321));
#28429=CARTESIAN_POINT('Ctrl Pts',(77.2207820174295,78.7571595604737,206.038134868243));
#28430=CARTESIAN_POINT('Ctrl Pts',(77.6211916289537,78.8069485066445,206.067174350675));
#28431=CARTESIAN_POINT('Ctrl Pts',(77.822008813833,78.8733824400182,206.082588569851));
#28432=CARTESIAN_POINT('Ctrl Pts',(78.1808309533484,79.0765901706023,206.111863297245));
#28433=CARTESIAN_POINT('Ctrl Pts',(78.3366632510614,79.2091600612225,206.124647668695));
#28434=CARTESIAN_POINT('Ctrl Pts',(78.5965453122727,79.5329154385169,206.152064544514));
#28435=CARTESIAN_POINT('Ctrl Pts',(78.6951616979899,79.7233173028714,206.16725414456));
#28436=CARTESIAN_POINT('Ctrl Pts',(78.8108803488985,80.1263876126478,206.197806251788));
#28437=CARTESIAN_POINT('Ctrl Pts',(78.8288516435248,80.3346609153489,206.212872334023));
#28438=CARTESIAN_POINT('Ctrl Pts',(78.7845858054451,80.744711603189,206.241162051983));
#28439=CARTESIAN_POINT('Ctrl Pts',(78.7234945932347,80.9426271118811,206.253538742612));
#28440=CARTESIAN_POINT('Ctrl Pts',(78.5262915101812,81.3112226257922,206.282498311826));
#28441=CARTESIAN_POINT('Ctrl Pts',(78.3895467147799,81.4768849140947,206.298051581849));
#28442=CARTESIAN_POINT('Ctrl Pts',(78.0655682483538,81.7399592826122,206.328384671391));
#28443=CARTESIAN_POINT('Ctrl Pts',(77.8833641244146,81.8373277503449,206.342897024088));
#28444=CARTESIAN_POINT('Ctrl Pts',(77.4852406403898,81.9602007489264,206.370081645795));
#28445=CARTESIAN_POINT('Ctrl Pts',(77.2723350705081,81.981867077468,206.383812602008));
#28446=CARTESIAN_POINT('Ctrl Pts',(76.8522474805038,81.9410988556117,206.414044114645));
#28447=CARTESIAN_POINT('Ctrl Pts',(76.6492066580898,81.8798372037296,206.429507893021));
#28448=CARTESIAN_POINT('Ctrl Pts',(76.2847596732123,81.68575826866,206.458989064702));
#28449=CARTESIAN_POINT('Ctrl Pts',(76.1255499030091,81.5572800398929,206.472088823458));
#28450=CARTESIAN_POINT('Ctrl Pts',(75.85739009848,81.2404453326028,206.499158009755));
#28451=CARTESIAN_POINT('Ctrl Pts',(75.7538709443149,81.0527025114772,206.514243701397));
#28452=CARTESIAN_POINT('Ctrl Pts',(75.6275459159743,80.6523209837157,206.54478808149));
#28453=CARTESIAN_POINT('Ctrl Pts',(75.6041976977911,80.4440461585913,206.559946930229));
#28454=CARTESIAN_POINT('Ctrl Pts',(75.6381324494241,80.0333725344831,206.58845881589));
#28455=CARTESIAN_POINT('Ctrl Pts',(75.693835156032,79.8348083827527,206.600780800812));
#28456=CARTESIAN_POINT('Ctrl Pts',(75.8809780090442,79.4613591540993,206.629454150093));
#28457=CARTESIAN_POINT('Ctrl Pts',(76.0136924153775,79.2917189964761,206.644995130815));
#28458=CARTESIAN_POINT('Ctrl Pts',(76.3316166364797,79.0197207198143,206.675458218143));
#28459=CARTESIAN_POINT('Ctrl Pts',(76.5117607144455,78.9175350303539,206.690104463321));
#28460=CARTESIAN_POINT('Ctrl Pts',(76.7496405829934,78.8376206949813,206.706674488704));
#28461=CARTESIAN_POINT('Ctrl Pts',(76.7934786972824,78.824957345521,206.70962421378));
#28462=CARTESIAN_POINT('Ctrl Pts',(76.8377292359504,78.814194574068,206.712499998088));
#28463=CARTESIAN_POINT('Ctrl Pts',(76.8377292359517,78.8141945740677,206.8));
#28464=CARTESIAN_POINT('Ctrl Pts',(76.7031628343352,78.8469242869579,206.791254706544));
#28465=CARTESIAN_POINT('Ctrl Pts',(76.573192662753,78.8970312216183,206.781876896184));
#28466=CARTESIAN_POINT('Ctrl Pts',(76.2676427912773,79.0633108488901,206.757389339445));
#28467=CARTESIAN_POINT('Ctrl Pts',(76.1055401402883,79.1980677513917,206.74205470168));
#28468=CARTESIAN_POINT('Ctrl Pts',(75.8401590437235,79.5248060945437,206.711606738352));
#28469=CARTESIAN_POINT('Ctrl Pts',(75.7404483387497,79.7144923942664,206.69679714349));
#28470=CARTESIAN_POINT('Ctrl Pts',(75.6233815825307,80.1132492705014,206.670545557463));
#28471=CARTESIAN_POINT('Ctrl Pts',(75.6037754590442,80.3176208162215,206.656411580955));
#28472=CARTESIAN_POINT('Ctrl Pts',(75.643046219008,80.7306773491343,206.626469338703));
#28473=CARTESIAN_POINT('Ctrl Pts',(75.7045291494201,80.9350293292451,206.610931265655));
#28474=CARTESIAN_POINT('Ctrl Pts',(75.9019114114379,81.3052993341646,206.58129581519));
#28475=CARTESIAN_POINT('Ctrl Pts',(76.0347618582989,81.468120535608,206.568444632706));
#28476=CARTESIAN_POINT('Ctrl Pts',(76.3536451345256,81.7323115455285,206.540714377177));
#28477=CARTESIAN_POINT('Ctrl Pts',(76.5360356092322,81.8318100281579,206.525911692908));
#28478=CARTESIAN_POINT('Ctrl Pts',(76.9361502253573,81.9586904897149,206.495312351129));
#28479=CARTESIAN_POINT('Ctrl Pts',(77.1510285772583,81.9818164417919,206.479802083691));
#28480=CARTESIAN_POINT('Ctrl Pts',(77.5668155004734,81.9431233309061,206.45150059773));
#28481=CARTESIAN_POINT('Ctrl Pts',(77.7640021649421,81.88577224502,206.439131629642));
#28482=CARTESIAN_POINT('Ctrl Pts',(78.130613908673,81.698012588912,206.410342008544));
#28483=CARTESIAN_POINT('Ctrl Pts',(78.2956834699523,81.5677700607989,206.395078184758));
#28484=CARTESIAN_POINT('Ctrl Pts',(78.5691662141335,81.2484118562036,206.364574506118));
#28485=CARTESIAN_POINT('Ctrl Pts',(78.6737920676496,81.0613408752536,206.349637353839));
#28486=CARTESIAN_POINT('Ctrl Pts',(78.8010612081228,80.6660762385,206.323023500772));
#28487=CARTESIAN_POINT('Ctrl Pts',(78.8259728468762,80.4627345162427,206.309396880066));
#28488=CARTESIAN_POINT('Ctrl Pts',(78.7978271852326,80.049796452476,206.279654746401));
#28489=CARTESIAN_POINT('Ctrl Pts',(78.7420885864796,79.8444095707088,206.264142339503));
#28490=CARTESIAN_POINT('Ctrl Pts',(78.5546369896886,79.467926160763,206.234237794231));
#28491=CARTESIAN_POINT('Ctrl Pts',(78.4251473336631,79.3004044864736,206.221047935949));
#28492=CARTESIAN_POINT('Ctrl Pts',(78.1121843959568,79.0276791522115,206.193556989518));
#28493=CARTESIAN_POINT('Ctrl Pts',(77.9328334352432,78.9238435470682,206.178878077657));
#28494=CARTESIAN_POINT('Ctrl Pts',(77.5371555125614,78.7870041470317,206.148385019757));
#28495=CARTESIAN_POINT('Ctrl Pts',(77.3235437267372,78.7582924327972,206.132848863259));
#28496=CARTESIAN_POINT('Ctrl Pts',(77.0183726466444,78.7784185326988,206.111907084985));
#28497=CARTESIAN_POINT('Ctrl Pts',(76.9271049840608,78.792456290664,206.10580841232));
#28498=CARTESIAN_POINT('Ctrl Pts',(76.8377292359512,78.8141945740679,206.1));
#28499=CARTESIAN_POINT('Origin',(77.215862801455,80.368869783441,212.));
#28500=CARTESIAN_POINT('',(76.8377292359514,78.8141945740678,207.5));
#28501=CARTESIAN_POINT('',(76.8377292359509,78.8141945740679,207.412499998088));
#28502=CARTESIAN_POINT('',(76.8377292359511,78.8141945740678,212.));
#28503=CARTESIAN_POINT('Ctrl Pts',(76.8377292359504,78.814194574068,206.712499998088));
#28504=CARTESIAN_POINT('Ctrl Pts',(76.997035119303,78.775447637528,206.722853077924));
#28505=CARTESIAN_POINT('Ctrl Pts',(77.161571312679,78.7613499102684,206.734077498517));
#28506=CARTESIAN_POINT('Ctrl Pts',(77.5358324712544,78.7871044077927,206.760794493322));
#28507=CARTESIAN_POINT('Ctrl Pts',(77.7410463522403,78.8429139599381,206.776298554896));
#28508=CARTESIAN_POINT('Ctrl Pts',(78.1112826620142,79.0274325164619,206.805988832192));
#28509=CARTESIAN_POINT('Ctrl Pts',(78.2740289188509,79.1517242309619,206.819498922382));
#28510=CARTESIAN_POINT('Ctrl Pts',(78.5506079792258,79.4613825138365,206.846204737318));
#28511=CARTESIAN_POINT('Ctrl Pts',(78.6590777580625,79.646263514295,206.861172978244));
#28512=CARTESIAN_POINT('Ctrl Pts',(78.7962154838579,80.0435947151159,206.891687570791));
#28513=CARTESIAN_POINT('Ctrl Pts',(78.8250902676227,80.2517283691258,206.906931654772));
#28514=CARTESIAN_POINT('Ctrl Pts',(78.8017416654103,80.6629722531716,206.935666371369));
#28515=CARTESIAN_POINT('Ctrl Pts',(78.7514710624391,80.8622346739487,206.948015477938));
#28516=CARTESIAN_POINT('Ctrl Pts',(78.5745460292897,81.2404883153497,206.976391813275));
#28517=CARTESIAN_POINT('Ctrl Pts',(78.4460225886296,81.4140566814621,206.991909535085));
#28518=CARTESIAN_POINT('Ctrl Pts',(78.134466906013,81.6949440521815,207.022484290718));
#28519=CARTESIAN_POINT('Ctrl Pts',(77.9565350789733,81.8019592720384,207.037257020441));
#28520=CARTESIAN_POINT('Ctrl Pts',(77.5671906874959,81.9436937733108,207.064928277103));
#28521=CARTESIAN_POINT('Ctrl Pts',(77.3591707612842,81.9760362641169,207.077855801554));
#28522=CARTESIAN_POINT('Ctrl Pts',(76.9397003487069,81.9589452951304,207.10755870483));
#28523=CARTESIAN_POINT('Ctrl Pts',(76.7324607878316,81.9086490494024,207.123091481919));
#28524=CARTESIAN_POINT('Ctrl Pts',(76.356505160668,81.7337516094761,207.152984720812));
#28525=CARTESIAN_POINT('Ctrl Pts',(76.1901980973244,81.6135807730318,207.166985795827));
#28526=CARTESIAN_POINT('Ctrl Pts',(75.9053941660867,81.3110660341237,207.193327219246));
#28527=CARTESIAN_POINT('Ctrl Pts',(75.7921319860464,81.1291329059222,207.208169185998));
#28528=CARTESIAN_POINT('Ctrl Pts',(75.6444236432481,80.7350919151538,207.238632823335));
#28529=CARTESIAN_POINT('Ctrl Pts',(75.6101008392802,80.5272387588863,207.25395091757));
#28530=CARTESIAN_POINT('Ctrl Pts',(75.6230304341367,80.1155061082904,207.282899810908));
#28531=CARTESIAN_POINT('Ctrl Pts',(75.668038150444,79.915511146734,207.295356861781));
#28532=CARTESIAN_POINT('Ctrl Pts',(75.8349977199822,79.5326927281716,207.323437427555));
#28533=CARTESIAN_POINT('Ctrl Pts',(75.9593452818444,79.3554057433861,207.33892213344));
#28534=CARTESIAN_POINT('Ctrl Pts',(76.2644868922184,79.0660278791462,207.369586086494));
#28535=CARTESIAN_POINT('Ctrl Pts',(76.4401486419303,78.9543692729348,207.3844728786));
#28536=CARTESIAN_POINT('Ctrl Pts',(76.6993146523219,78.8528307943672,207.403254352416));
#28537=CARTESIAN_POINT('Ctrl Pts',(76.7679808517075,78.8311590210875,207.407967142331));
#28538=CARTESIAN_POINT('Ctrl Pts',(76.8377292359507,78.814194574068,207.412499998088));
#28539=CARTESIAN_POINT('Ctrl Pts',(76.8377292359517,78.8141945740677,207.5));
#28540=CARTESIAN_POINT('Ctrl Pts',(76.6777981233889,78.8530935810524,207.48960628734));
#28541=CARTESIAN_POINT('Ctrl Pts',(76.5246335080535,78.9164726848852,207.47833689724));
#28542=CARTESIAN_POINT('Ctrl Pts',(76.2044243933626,79.111483892041,207.451629555803));
#28543=CARTESIAN_POINT('Ctrl Pts',(76.0484270350896,79.2548152912046,207.436185205297));
#28544=CARTESIAN_POINT('Ctrl Pts',(75.7989033333978,79.5958868983958,207.405851928815));
#28545=CARTESIAN_POINT('Ctrl Pts',(75.7088299834789,79.7908829252769,207.391921163592));
#28546=CARTESIAN_POINT('Ctrl Pts',(75.6120532891954,80.1967064537015,207.364835845637));
#28547=CARTESIAN_POINT('Ctrl Pts',(75.6032112991938,80.4028991933799,207.350379237481));
#28548=CARTESIAN_POINT('Ctrl Pts',(75.6647703143932,80.8152443372814,207.320103312222));
#28549=CARTESIAN_POINT('Ctrl Pts',(75.737685014966,81.0170576733383,207.304548105169));
#28550=CARTESIAN_POINT('Ctrl Pts',(75.9545984511083,81.3746174799975,207.275476612147));
#28551=CARTESIAN_POINT('Ctrl Pts',(76.0941610081724,81.5282219652729,207.263055990249));
#28552=CARTESIAN_POINT('Ctrl Pts',(76.4248741664475,81.7749838042379,207.234855263202));
#28553=CARTESIAN_POINT('Ctrl Pts',(76.6131380772798,81.8653711679294,207.219828377068));
#28554=CARTESIAN_POINT('Ctrl Pts',(77.0188179295303,81.9708193125118,207.189279004408));
#28555=CARTESIAN_POINT('Ctrl Pts',(77.2329191960042,81.9828143537899,207.174051315461));
#28556=CARTESIAN_POINT('Ctrl Pts',(77.6439443479865,81.9238277299733,207.146499085306));
#28557=CARTESIAN_POINT('Ctrl Pts',(77.8374137083549,81.8571059993959,207.13381639049));
#28558=CARTESIAN_POINT('Ctrl Pts',(78.1947768040688,81.6516537639493,207.104623754626));
#28559=CARTESIAN_POINT('Ctrl Pts',(78.3540002206048,81.5127417182456,207.089231765731));
#28560=CARTESIAN_POINT('Ctrl Pts',(78.6118112428972,81.1790752348933,207.058834239073));
#28561=CARTESIAN_POINT('Ctrl Pts',(78.7068414276177,80.9869296971543,207.044483726747));
#28562=CARTESIAN_POINT('Ctrl Pts',(78.8142904703869,80.5848573721532,207.01784809846));
#28563=CARTESIAN_POINT('Ctrl Pts',(78.828767629234,80.3795513980379,207.003551427495));
#28564=CARTESIAN_POINT('Ctrl Pts',(78.7789410778507,79.9667873192257,206.97344800168));
#28565=CARTESIAN_POINT('Ctrl Pts',(78.7120246101494,79.7635618210616,206.957896106856));
#28566=CARTESIAN_POINT('Ctrl Pts',(78.5053254270433,79.399274287447,206.92852396573));
#28567=CARTESIAN_POINT('Ctrl Pts',(78.3692935007023,79.2408549348209,206.91591869202));
#28568=CARTESIAN_POINT('Ctrl Pts',(78.0447982122093,78.9848685281713,206.887963942756));
#28569=CARTESIAN_POINT('Ctrl Pts',(77.859585667051,78.8896185850703,206.873050885631));
#28570=CARTESIAN_POINT('Ctrl Pts',(77.455439567366,78.7724342951044,206.84236822745));
#28571=CARTESIAN_POINT('Ctrl Pts',(77.239477261348,78.7547193693666,206.826893045004));
#28572=CARTESIAN_POINT('Ctrl Pts',(76.9627741045119,78.7877137527686,206.808207135088));
#28573=CARTESIAN_POINT('Ctrl Pts',(76.899771582067,78.7991044167105,206.804032050474));
#28574=CARTESIAN_POINT('Ctrl Pts',(76.8377292359517,78.8141945740677,206.8));
#28575=CARTESIAN_POINT('Origin',(77.215862801455,80.368869783441,212.));
#28576=CARTESIAN_POINT('',(76.8377292359511,78.8141945740678,208.2));
#28577=CARTESIAN_POINT('',(76.8377292359511,78.8141945740679,208.112499998088));
#28578=CARTESIAN_POINT('',(76.8377292359511,78.8141945740678,212.));
#28579=CARTESIAN_POINT('Ctrl Pts',(76.8377292359507,78.814194574068,207.412499998088));
#28580=CARTESIAN_POINT('Ctrl Pts',(76.9684916976914,78.7823900687964,207.420998078495));
#28581=CARTESIAN_POINT('Ctrl Pts',(77.1029799634108,78.7671439496196,207.430096346542));
#28582=CARTESIAN_POINT('Ctrl Pts',(77.4498635404948,78.7719712833825,207.454468549654));
#28583=CARTESIAN_POINT('Ctrl Pts',(77.658907610699,78.8169227172997,207.470018020224));
#28584=CARTESIAN_POINT('Ctrl Pts',(78.0400365892561,78.9824124890444,207.500080392696));
#28585=CARTESIAN_POINT('Ctrl Pts',(78.2097935453799,79.0985650149274,207.514340479469));
#28586=CARTESIAN_POINT('Ctrl Pts',(78.5024133351802,79.394297461228,207.540879594097));
#28587=CARTESIAN_POINT('Ctrl Pts',(78.6202345840811,79.5733568839449,207.555338093668));
#28588=CARTESIAN_POINT('Ctrl Pts',(78.777931269987,79.9642816395426,207.585753067982));
#28589=CARTESIAN_POINT('Ctrl Pts',(78.817392852367,80.1717416404156,207.601131861497));
#28590=CARTESIAN_POINT('Ctrl Pts',(78.8142889134598,80.5838686624257,207.630278018563));
#28591=CARTESIAN_POINT('Ctrl Pts',(78.7741757834228,80.7845972519932,207.642908972068));
#28592=CARTESIAN_POINT('Ctrl Pts',(78.6174978654381,81.169200555034,207.670537125653));
#28593=CARTESIAN_POINT('Ctrl Pts',(78.4990185776205,81.3479424802035,207.685785579469));
#28594=CARTESIAN_POINT('Ctrl Pts',(78.2032078888692,81.6447597587104,207.716331966708));
#28595=CARTESIAN_POINT('Ctrl Pts',(78.0302282929965,81.7615583376688,207.731336090101));
#28596=CARTESIAN_POINT('Ctrl Pts',(77.6501511969106,81.922511869429,207.759486234002));
#28597=CARTESIAN_POINT('Ctrl Pts',(77.4468528725997,81.9654469115731,207.771937330493));
#28598=CARTESIAN_POINT('Ctrl Pts',(77.0285798523411,81.9720006089835,207.801071691852));
#28599=CARTESIAN_POINT('Ctrl Pts',(76.8177006931565,81.9330156752873,207.816627250096));
#28600=CARTESIAN_POINT('Ctrl Pts',(76.4309339806257,81.7779981310026,207.846869426193));
#28601=CARTESIAN_POINT('Ctrl Pts',(76.2575180542302,81.6663189293149,207.861293839571));
#28602=CARTESIAN_POINT('Ctrl Pts',(75.9558238922242,81.3776835173705,207.888322434105));
#28603=CARTESIAN_POINT('Ctrl Pts',(75.8327778251431,81.2010625880721,207.902372454566));
#28604=CARTESIAN_POINT('Ctrl Pts',(75.6645181565862,80.8130528558924,207.932762924489));
#28605=CARTESIAN_POINT('Ctrl Pts',(75.6197177765441,80.606133740526,207.948195397308));
#28606=CARTESIAN_POINT('Ctrl Pts',(75.6126023097434,80.1936661904108,207.977541788595));
#28607=CARTESIAN_POINT('Ctrl Pts',(75.6476879821394,79.9921297253142,207.990425839145));
#28608=CARTESIAN_POINT('Ctrl Pts',(75.7946267510987,79.6038939155045,208.017723220263));
#28609=CARTESIAN_POINT('Ctrl Pts',(75.9085760800567,79.4222656484567,208.032878078399));
#28610=CARTESIAN_POINT('Ctrl Pts',(76.1971711430594,79.1177820053721,208.06342989267));
#28611=CARTESIAN_POINT('Ctrl Pts',(76.3676404318543,78.9964647868572,208.078529127192));
#28612=CARTESIAN_POINT('Ctrl Pts',(76.6472679322046,78.8699976331339,208.099644936608));
#28613=CARTESIAN_POINT('Ctrl Pts',(76.7414060787578,78.8376226307131,208.106240082789));
#28614=CARTESIAN_POINT('Ctrl Pts',(76.8377292359511,78.8141945740679,208.112499998088));
#28615=CARTESIAN_POINT('Ctrl Pts',(76.8377292359511,78.8141945740679,208.2));
#28616=CARTESIAN_POINT('Ctrl Pts',(76.6496783488809,78.8599329713841,208.187778820179));
#28617=CARTESIAN_POINT('Ctrl Pts',(76.4713255474108,78.9394459630036,208.174368609384));
#28618=CARTESIAN_POINT('Ctrl Pts',(76.137386981879,79.1682907824281,208.145233638291));
#28619=CARTESIAN_POINT('Ctrl Pts',(75.9886585518949,79.3207877535425,208.12971118779));
#28620=CARTESIAN_POINT('Ctrl Pts',(75.759870735986,79.6732601904406,208.099897548496));
#28621=CARTESIAN_POINT('Ctrl Pts',(75.6815085293303,79.869351520945,208.08683239959));
#28622=CARTESIAN_POINT('Ctrl Pts',(75.6053274043631,80.2770487558979,208.05925941127));
#28623=CARTESIAN_POINT('Ctrl Pts',(75.6068699396097,80.4844616896433,208.044537398159));
#28624=CARTESIAN_POINT('Ctrl Pts',(75.6898899419757,80.8951932736331,208.014005965699));
#28625=CARTESIAN_POINT('Ctrl Pts',(75.7736942510371,81.0939820127701,207.998477397809));
#28626=CARTESIAN_POINT('Ctrl Pts',(76.0090201561273,81.438982522867,207.969978448938));
#28627=CARTESIAN_POINT('Ctrl Pts',(76.1550860915338,81.5839284341693,207.957650674205));
#28628=CARTESIAN_POINT('Ctrl Pts',(76.4971871757524,81.813428594404,207.929006967727));
#28629=CARTESIAN_POINT('Ctrl Pts',(76.6908018298294,81.8944966741833,207.913796722969));
#28630=CARTESIAN_POINT('Ctrl Pts',(77.1023676486615,81.9788871083084,207.883267196219));
#28631=CARTESIAN_POINT('Ctrl Pts',(77.3167345151289,81.9797418516438,207.868249316131));
#28632=CARTESIAN_POINT('Ctrl Pts',(77.7240333610203,81.899519390134,207.841393204133));
#28633=CARTESIAN_POINT('Ctrl Pts',(77.9138050455682,81.8228515260244,207.828062625307));
#28634=CARTESIAN_POINT('Ctrl Pts',(78.260956467854,81.5985201212301,207.798458022898));
#28635=CARTESIAN_POINT('Ctrl Pts',(78.4134136759075,81.4505971161129,207.78296920396));
#28636=CARTESIAN_POINT('Ctrl Pts',(78.6526610489904,81.1037890896475,207.752889101302));
#28637=CARTESIAN_POINT('Ctrl Pts',(78.7368891754549,80.9082538630004,207.739427260937));
#28638=CARTESIAN_POINT('Ctrl Pts',(78.8234897447539,80.5014693206156,207.712098492507));
#28639=CARTESIAN_POINT('Ctrl Pts',(78.8272266223828,80.2946102882477,207.69750670218));
#28640=CARTESIAN_POINT('Ctrl Pts',(78.7550916221485,79.8829233435445,207.667095158804));
#28641=CARTESIAN_POINT('Ctrl Pts',(78.6767972232593,79.6825291409411,207.651547792439));
#28642=CARTESIAN_POINT('Ctrl Pts',(78.4507725554193,79.3311185265315,207.622754965691));
#28643=CARTESIAN_POINT('Ctrl Pts',(78.30801310448,79.1817987667151,207.610419838608));
#28644=CARTESIAN_POINT('Ctrl Pts',(77.9716950288724,78.9434768952379,207.581999939645));
#28645=CARTESIAN_POINT('Ctrl Pts',(77.7807557196506,78.8576117586452,207.566878555098));
#28646=CARTESIAN_POINT('Ctrl Pts',(77.3720576160872,78.7624273203424,207.536328402515));
#28647=CARTESIAN_POINT('Ctrl Pts',(77.1577516537931,78.755884884644,207.521198177244));
#28648=CARTESIAN_POINT('Ctrl Pts',(76.9111913140107,78.7976925211682,207.504802201921));
#28649=CARTESIAN_POINT('Ctrl Pts',(76.8742863805139,78.8053030169537,207.502375800744));
#28650=CARTESIAN_POINT('Ctrl Pts',(76.8377292359517,78.8141945740677,207.5));
#28651=CARTESIAN_POINT('Origin',(77.215862801455,80.368869783441,212.));
#28652=CARTESIAN_POINT('',(76.8377292359511,78.8141945740679,208.9));
#28653=CARTESIAN_POINT('',(76.8377292359513,78.8141945740678,208.812499998088));
#28654=CARTESIAN_POINT('',(76.8377292359511,78.8141945740678,212.));
#28655=CARTESIAN_POINT('Ctrl Pts',(76.8377292359511,78.8141945740679,208.112499998088));
#28656=CARTESIAN_POINT('Ctrl Pts',(76.9396630831313,78.7894018656955,208.11912454475));
#28657=CARTESIAN_POINT('Ctrl Pts',(77.0439972318632,78.7746397691921,208.126122696795));
#28658=CARTESIAN_POINT('Ctrl Pts',(77.3620334959564,78.7613966957854,208.148105831678));
#28659=CARTESIAN_POINT('Ctrl Pts',(77.574385754742,78.7950926560753,208.163656037733));
#28660=CARTESIAN_POINT('Ctrl Pts',(77.9658637169711,78.9407742712014,208.194036482534));
#28661=CARTESIAN_POINT('Ctrl Pts',(78.1423918359513,79.0484372526846,208.208596333037));
#28662=CARTESIAN_POINT('Ctrl Pts',(78.4499527939014,79.3288435688161,208.235866747699));
#28663=CARTESIAN_POINT('Ctrl Pts',(78.5763638298165,79.5007032173591,208.249434493321));
#28664=CARTESIAN_POINT('Ctrl Pts',(78.754662616906,79.8827631611168,208.279576414897));
#28665=CARTESIAN_POINT('Ctrl Pts',(78.805155940984,80.088956282147,208.29505555474));
#28666=CARTESIAN_POINT('Ctrl Pts',(78.8231964431696,80.5017076070801,208.324610319086));
#28667=CARTESIAN_POINT('Ctrl Pts',(78.7934223240728,80.7041582210938,208.337843799841));
#28668=CARTESIAN_POINT('Ctrl Pts',(78.6567644858968,81.0961177626275,208.364786426685));
#28669=CARTESIAN_POINT('Ctrl Pts',(78.5476612347784,81.2806560417358,208.379832208013));
#28670=CARTESIAN_POINT('Ctrl Pts',(78.2668783640649,81.5930182716591,208.410368670172));
#28671=CARTESIAN_POINT('Ctrl Pts',(78.0991775394105,81.7190355748876,208.425558535636));
#28672=CARTESIAN_POINT('Ctrl Pts',(77.7282312102709,81.8983015302319,208.454149120467));
#28673=CARTESIAN_POINT('Ctrl Pts',(77.5291678402495,81.9511212129701,208.466471027369));
#28674=CARTESIAN_POINT('Ctrl Pts',(77.112500469628,81.9797377129393,208.495040709726));
#28675=CARTESIAN_POINT('Ctrl Pts',(76.898754559665,81.9515872121988,208.51057474579));
#28676=CARTESIAN_POINT('Ctrl Pts',(76.5026180724941,81.8157460596159,208.541079426116));
#28677=CARTESIAN_POINT('Ctrl Pts',(76.3229558484872,81.7123439487735,208.555771231337));
#28678=CARTESIAN_POINT('Ctrl Pts',(76.0093919016011,81.4404794011624,208.583286585955));
#28679=CARTESIAN_POINT('Ctrl Pts',(75.8795605854027,81.27343750618,208.596438422272));
#28680=CARTESIAN_POINT('Ctrl Pts',(75.6910960792052,80.8975801057865,208.626316069202));
#28681=CARTESIAN_POINT('Ctrl Pts',(75.6347740023039,80.692291073723,208.641831598217));
#28682=CARTESIAN_POINT('Ctrl Pts',(75.6055013609186,80.2793368025846,208.671594301038));
#28683=CARTESIAN_POINT('Ctrl Pts',(75.6298734058512,80.0758930474358,208.68526881607));
#28684=CARTESIAN_POINT('Ctrl Pts',(75.7561026578783,79.6802677912866,208.711845979796));
#28685=CARTESIAN_POINT('Ctrl Pts',(75.860229790237,79.492923688012,208.726770579827));
#28686=CARTESIAN_POINT('Ctrl Pts',(76.1328946305887,79.1728025539968,208.757269533244));
#28687=CARTESIAN_POINT('Ctrl Pts',(76.2976668473919,79.0420961464191,208.772541030412));
#28688=CARTESIAN_POINT('Ctrl Pts',(76.5957546958503,78.8884667952882,208.795998086802));
#28689=CARTESIAN_POINT('Ctrl Pts',(76.7148672649924,78.8440774942195,208.804515360187));
#28690=CARTESIAN_POINT('Ctrl Pts',(76.8377292359514,78.8141945740678,208.812499998088));
#28691=CARTESIAN_POINT('Ctrl Pts',(76.837729235951,78.8141945740679,208.9));
#28692=CARTESIAN_POINT('Ctrl Pts',(76.8191600495721,78.8187110368066,208.898793213));
#28693=CARTESIAN_POINT('Ctrl Pts',(76.8006598466345,78.8235630882186,208.897573167653));
#28694=CARTESIAN_POINT('Ctrl Pts',(76.5856257667561,78.8841065309996,208.883183400459));
#28695=CARTESIAN_POINT('Ctrl Pts',(76.4014766339768,78.9765868869151,208.868814576868));
#28696=CARTESIAN_POINT('Ctrl Pts',(76.0716504374976,79.2305489188511,208.838631864517));
#28697=CARTESIAN_POINT('Ctrl Pts',(75.9309645086107,79.3921155504159,208.823076943288));
#28698=CARTESIAN_POINT('Ctrl Pts',(75.7236729500161,79.7557136693539,208.793836898622));
#28699=CARTESIAN_POINT('Ctrl Pts',(75.657130075,79.953013318426,208.781324975927));
#28700=CARTESIAN_POINT('Ctrl Pts',(75.6025894183993,80.362378866944,208.753260863177));
#28701=CARTESIAN_POINT('Ctrl Pts',(75.6152367173269,80.5705151760514,208.738296233638));
#28702=CARTESIAN_POINT('Ctrl Pts',(75.7203694459341,80.9759750235647,208.70775724856));
#28703=CARTESIAN_POINT('Ctrl Pts',(75.8140473721468,81.1688867810982,208.692474922603));
#28704=CARTESIAN_POINT('Ctrl Pts',(76.065636006685,81.4994404471978,208.66471929837));
#28705=CARTESIAN_POINT('Ctrl Pts',(76.2181757101933,81.6360911709214,208.652166546734));
#28706=CARTESIAN_POINT('Ctrl Pts',(76.5714307894876,81.8481880514375,208.623099133227));
#28707=CARTESIAN_POINT('Ctrl Pts',(76.7699443474843,81.9196185486146,208.607743673018));
#28708=CARTESIAN_POINT('Ctrl Pts',(77.1865225688845,81.9826337295144,208.577301630105));
#28709=CARTESIAN_POINT('Ctrl Pts',(77.4005921695774,81.9722594527818,208.562653369994));
#28710=CARTESIAN_POINT('Ctrl Pts',(77.8038082113088,81.8708052628951,208.536278579317));
#28711=CARTESIAN_POINT('Ctrl Pts',(77.9899853334896,81.783852779215,208.522081119817));
#28712=CARTESIAN_POINT('Ctrl Pts',(78.3260756228065,81.5402632488109,208.492090273253));
#28713=CARTESIAN_POINT('Ctrl Pts',(78.471043211573,81.3833983407653,208.476546255731));
#28714=CARTESIAN_POINT('Ctrl Pts',(78.689613075432,81.0255537745091,208.447001053133));
#28715=CARTESIAN_POINT('Ctrl Pts',(78.7623199526234,80.8289024317685,208.434243365705));
#28716=CARTESIAN_POINT('Ctrl Pts',(78.8282550590881,80.4203772188331,208.406435148202));
#28717=CARTESIAN_POINT('Ctrl Pts',(78.8214758388479,80.2125490428189,208.39159347277));
#28718=CARTESIAN_POINT('Ctrl Pts',(78.7277105333233,79.8030377521981,208.360963329375));
#28719=CARTESIAN_POINT('Ctrl Pts',(78.6384938779096,79.6059784248178,208.345464023115));
#28720=CARTESIAN_POINT('Ctrl Pts',(78.3940524213567,79.2673983913106,208.317262886865));
#28721=CARTESIAN_POINT('Ctrl Pts',(78.2446827883486,79.1267307472499,208.304859305263));
#28722=CARTESIAN_POINT('Ctrl Pts',(77.8968581088172,78.9060952802595,208.275996829927));
#28723=CARTESIAN_POINT('Ctrl Pts',(77.70068443458,78.8299098716014,208.260707620031));
#28724=CARTESIAN_POINT('Ctrl Pts',(77.2865362487069,78.7564111077173,208.230220688716));
#28725=CARTESIAN_POINT('Ctrl Pts',(77.0722643830667,78.7612479163064,208.215326142416));
#28726=CARTESIAN_POINT('Ctrl Pts',(76.8559773625412,78.8098410641186,208.201187661587));
#28727=CARTESIAN_POINT('Ctrl Pts',(76.846842092359,78.8119781131218,208.200592232552));
#28728=CARTESIAN_POINT('Ctrl Pts',(76.8377292359511,78.8141945740679,208.2));
#28729=CARTESIAN_POINT('Origin',(77.215862801455,80.368869783441,212.));
#28730=CARTESIAN_POINT('',(76.8377292359507,78.8141945740679,209.6));
#28731=CARTESIAN_POINT('',(76.8377292359515,78.8141945740678,209.512499998088));
#28732=CARTESIAN_POINT('',(76.8377292359511,78.8141945740678,212.));
#28733=CARTESIAN_POINT('Ctrl Pts',(76.8377292359514,78.8141945740678,208.812499998088));
#28734=CARTESIAN_POINT('Ctrl Pts',(76.9117861001804,78.7961822034118,208.817312856293));
#28735=CARTESIAN_POINT('Ctrl Pts',(76.9871810149374,78.7834478133498,208.822327552005));
#28736=CARTESIAN_POINT('Ctrl Pts',(77.2764642233986,78.7557509783693,208.842002361462));
#28737=CARTESIAN_POINT('Ctrl Pts',(77.4914599607559,78.7783229727028,208.857509485931));
#28738=CARTESIAN_POINT('Ctrl Pts',(77.891999254429,78.904212966651,208.888118238391));
#28739=CARTESIAN_POINT('Ctrl Pts',(78.0746841308784,79.0032786127344,208.902932649615));
#28740=CARTESIAN_POINT('Ctrl Pts',(78.3941473199926,79.2666270286464,208.930686210092));
#28741=CARTESIAN_POINT('Ctrl Pts',(78.5273265651122,79.4289909173781,208.943508557155));
#28742=CARTESIAN_POINT('Ctrl Pts',(78.7256759252887,79.7986468145787,208.973117163087));
#28743=CARTESIAN_POINT('Ctrl Pts',(78.7877209789437,80.0028889353391,208.988657139353));
#28744=CARTESIAN_POINT('Ctrl Pts',(78.8280647507798,80.4157520639106,209.018604169536));
#28745=CARTESIAN_POINT('Ctrl Pts',(78.8090546736185,80.6202277288121,209.032763898));
#28746=CARTESIAN_POINT('Ctrl Pts',(78.6929807637921,81.0193264871479,209.059040216555));
#28747=CARTESIAN_POINT('Ctrl Pts',(78.5938153353027,81.2093094331402,209.07380566194));
#28748=CARTESIAN_POINT('Ctrl Pts',(78.3290952503072,81.5369145567883,209.104262403781));
#28749=CARTESIAN_POINT('Ctrl Pts',(78.1672858277899,81.672104377895,209.119603373155));
#28750=CARTESIAN_POINT('Ctrl Pts',(77.8058893717694,81.8699115993271,209.148623816298));
#28751=CARTESIAN_POINT('Ctrl Pts',(77.6108449824573,81.9325932893769,209.161135508644));
#28752=CARTESIAN_POINT('Ctrl Pts',(77.1984050893787,81.982812432269,209.188966483185));
#28753=CARTESIAN_POINT('Ctrl Pts',(76.9845865057771,81.9662399063241,209.204268237249));
#28754=CARTESIAN_POINT('Ctrl Pts',(76.5816439968789,81.8522386682799,209.234801416215));
#28755=CARTESIAN_POINT('Ctrl Pts',(76.395709763203,81.7581123737807,209.249741936985));
#28756=CARTESIAN_POINT('Ctrl Pts',(76.0697589604614,81.504272494516,209.277754528787));
#28757=CARTESIAN_POINT('Ctrl Pts',(75.9329015039603,81.3469861040627,209.290308219051));
#28758=CARTESIAN_POINT('Ctrl Pts',(75.7238011499693,80.9842642711913,209.319610807118));
#28759=CARTESIAN_POINT('Ctrl Pts',(75.6554782008993,80.7813539375629,209.335164609594));
#28760=CARTESIAN_POINT('Ctrl Pts',(75.602906180264,80.3686585369461,209.365310481194));
#28761=CARTESIAN_POINT('Ctrl Pts',(75.6160673347275,80.1631311343417,209.379645518849));
#28762=CARTESIAN_POINT('Ctrl Pts',(75.721542016164,79.758184447611,209.406518822256));
#28763=CARTESIAN_POINT('Ctrl Pts',(75.8167054451588,79.5636534840546,209.420913789842));
#28764=CARTESIAN_POINT('Ctrl Pts',(76.0750556983137,79.2276515583953,209.451457345137));
#28765=CARTESIAN_POINT('Ctrl Pts',(76.2339935886625,79.0883386734642,209.466854456699));
#28766=CARTESIAN_POINT('Ctrl Pts',(76.5475346151698,78.9071303852898,209.492515136969));
#28767=CARTESIAN_POINT('Ctrl Pts',(76.6897902221338,78.8501768206713,209.502885636153));
#28768=CARTESIAN_POINT('Ctrl Pts',(76.8377292359518,78.8141945740677,209.512499998088));
#28769=CARTESIAN_POINT('Ctrl Pts',(76.8377292359504,78.814194574068,209.6));
#28770=CARTESIAN_POINT('Ctrl Pts',(76.7942908559166,78.8247598094451,209.597176996813));
#28771=CARTESIAN_POINT('Ctrl Pts',(76.7512492262698,78.8371566672181,209.594282698051));
#28772=CARTESIAN_POINT('Ctrl Pts',(76.5140714446782,78.9164207692148,209.577782441394));
#28773=CARTESIAN_POINT('Ctrl Pts',(76.3337928147036,79.0183018514361,209.563144436412));
#28774=CARTESIAN_POINT('Ctrl Pts',(76.0154770429867,79.2897375258994,209.532689024434));
#28775=CARTESIAN_POINT('Ctrl Pts',(75.8825033975968,79.4591278980739,209.517146947354));
#28776=CARTESIAN_POINT('Ctrl Pts',(75.6947207488768,79.8322719764637,209.488455217788));
#28777=CARTESIAN_POINT('Ctrl Pts',(75.6386764922219,80.0307940860058,209.476132128372));
#28778=CARTESIAN_POINT('Ctrl Pts',(75.604082006991,80.4414297232222,209.447634303082));
#28779=CARTESIAN_POINT('Ctrl Pts',(75.6270862834564,80.6497085558458,209.432481097433));
#28780=CARTESIAN_POINT('Ctrl Pts',(75.752735412568,81.0502703273327,209.401935594412));
#28781=CARTESIAN_POINT('Ctrl Pts',(75.855943501156,81.2381869490555,209.386842949294));
#28782=CARTESIAN_POINT('Ctrl Pts',(76.1235765041631,81.5554660965533,209.359751352111));
#28783=CARTESIAN_POINT('Ctrl Pts',(76.2825684687308,81.6842053783251,209.346674233288));
#28784=CARTESIAN_POINT('Ctrl Pts',(76.6466554791337,81.8788731444417,209.317206178883));
#28785=CARTESIAN_POINT('Ctrl Pts',(76.8495572389379,81.9404695091472,209.301745269278));
#28786=CARTESIAN_POINT('Ctrl Pts',(77.269654312385,81.981974038721,209.271497997527));
#28787=CARTESIAN_POINT('Ctrl Pts',(77.4827137482154,81.9606415523302,209.257737116563));
#28788=CARTESIAN_POINT('Ctrl Pts',(77.8811026128087,81.8383493555527,209.230567741071));
#28789=CARTESIAN_POINT('Ctrl Pts',(78.0634291017205,81.7412780091156,209.216063894433));
#28790=CARTESIAN_POINT('Ctrl Pts',(78.3877714364682,81.4787559021546,209.185739419629));
#28791=CARTESIAN_POINT('Ctrl Pts',(78.5247600209496,81.3133408784821,209.170185741196));
#28792=CARTESIAN_POINT('Ctrl Pts',(78.7225796795045,80.9450468700421,209.141208832876));
#28793=CARTESIAN_POINT('Ctrl Pts',(78.7840025383195,80.7471701291659,209.128826191886));
#28794=CARTESIAN_POINT('Ctrl Pts',(78.8288986903484,80.3371594828524,209.100550172892));
#28795=CARTESIAN_POINT('Ctrl Pts',(78.8112547470093,80.1288907067295,209.085490052499));
#28796=CARTESIAN_POINT('Ctrl Pts',(78.6961845719065,79.7256656223808,209.054938154282));
#28797=CARTESIAN_POINT('Ctrl Pts',(78.5978694193352,79.5351058904301,209.03974256019));
#28798=CARTESIAN_POINT('Ctrl Pts',(78.3384943630141,79.2109310072873,209.012304698965));
#28799=CARTESIAN_POINT('Ctrl Pts',(78.1828658951182,79.0781111608098,208.999536877318));
#28800=CARTESIAN_POINT('Ctrl Pts',(77.8243860671525,78.8743527481466,208.97027481335));
#28801=CARTESIAN_POINT('Ctrl Pts',(77.623707638452,78.8076080485544,208.954863932446));
#28802=CARTESIAN_POINT('Ctrl Pts',(77.2225449303185,78.7570603845167,208.925756197003));
#28803=CARTESIAN_POINT('Ctrl Pts',(77.0266459230265,78.7682455938331,208.912277447025));
#28804=CARTESIAN_POINT('Ctrl Pts',(76.837729235951,78.8141945740679,208.9));
#28805=CARTESIAN_POINT('Origin',(77.215862801455,80.368869783441,212.));
#28806=CARTESIAN_POINT('',(76.8377292359509,78.8141945740679,210.3));
#28807=CARTESIAN_POINT('',(76.8377292359512,78.8141945740678,210.212499998088));
#28808=CARTESIAN_POINT('',(76.8377292359511,78.8141945740678,212.));
#28809=CARTESIAN_POINT('Ctrl Pts',(76.8377292359518,78.8141945740677,209.512499998088));
#28810=CARTESIAN_POINT('Ctrl Pts',(76.8862442835823,78.802394573765,209.515652927225));
#28811=CARTESIAN_POINT('Ctrl Pts',(76.935360342617,78.7928534801644,209.518894223502));
#28812=CARTESIAN_POINT('Ctrl Pts',(77.1950863244861,78.754969094926,209.536291899824));
#28813=CARTESIAN_POINT('Ctrl Pts',(77.4092120307742,78.7664703996703,209.551511176548));
#28814=CARTESIAN_POINT('Ctrl Pts',(77.8151760340083,78.8709925406764,209.582061448137));
#28815=CARTESIAN_POINT('Ctrl Pts',(78.0036866632141,78.9609734855733,209.597097266181));
#28816=CARTESIAN_POINT('Ctrl Pts',(78.334910275856,79.2069716197041,209.625318055162));
#28817=CARTESIAN_POINT('Ctrl Pts',(78.4747632965217,79.3601837318022,209.637727689104));
#28818=CARTESIAN_POINT('Ctrl Pts',(78.6925102643476,79.7171867555457,209.666774097412));
#28819=CARTESIAN_POINT('Ctrl Pts',(78.7659160943085,79.9188765542249,209.682329015168));
#28820=CARTESIAN_POINT('Ctrl Pts',(78.8284385204956,80.3311727507581,209.712618074578));
#28821=CARTESIAN_POINT('Ctrl Pts',(78.8200605799987,80.5374314086927,209.727087349915));
#28822=CARTESIAN_POINT('Ctrl Pts',(78.7242133712058,80.9433456001172,209.75419510894));
#28823=CARTESIAN_POINT('Ctrl Pts',(78.6346787952959,81.1383909680076,209.768079714338));
#28824=CARTESIAN_POINT('Ctrl Pts',(78.3860960677452,81.479995141551,209.798390175903));
#28825=CARTESIAN_POINT('Ctrl Pts',(78.2304176921289,81.623750918391,209.813839069646));
#28826=CARTESIAN_POINT('Ctrl Pts',(77.8784595048441,81.8392798590798,209.843253993662));
#28827=CARTESIAN_POINT('Ctrl Pts',(77.6869965317385,81.9113133854704,209.856243064268));
#28828=CARTESIAN_POINT('Ctrl Pts',(77.2779212303413,81.9817072837881,209.883424985593));
#28829=CARTESIAN_POINT('Ctrl Pts',(77.0636031282149,81.9756895263487,209.898545303591));
#28830=CARTESIAN_POINT('Ctrl Pts',(76.6546284829339,81.8814970527803,209.929094470332));
#28831=CARTESIAN_POINT('Ctrl Pts',(76.4634374439547,81.7960710115093,209.944224467541));
#28832=CARTESIAN_POINT('Ctrl Pts',(76.1265830158737,81.5585617417386,209.972665238197));
#28833=CARTESIAN_POINT('Ctrl Pts',(75.9835180214879,81.4096499123308,209.984996163619));
#28834=CARTESIAN_POINT('Ctrl Pts',(75.7566267729065,81.0588304429404,210.013762040584));
#28835=CARTESIAN_POINT('Ctrl Pts',(75.677819786164,80.8585790697991,210.029308120574));
#28836=CARTESIAN_POINT('Ctrl Pts',(75.6046744280676,80.4469689261906,210.059731633652));
#28837=CARTESIAN_POINT('Ctrl Pts',(75.6079223383217,80.2400528448175,210.074335892166));
#28838=CARTESIAN_POINT('Ctrl Pts',(75.6935536740291,79.8331803748162,210.101687592826));
#28839=CARTESIAN_POINT('Ctrl Pts',(75.7772311264332,79.6375937389282,210.115108963578));
#28840=CARTESIAN_POINT('Ctrl Pts',(76.0155027725043,79.2902500026941,210.145164576635));
#28841=CARTESIAN_POINT('Ctrl Pts',(76.1676174268031,79.141896015853,210.160657028122));
#28842=CARTESIAN_POINT('Ctrl Pts',(76.4956184297709,78.9287615566256,210.188687829182));
#28843=CARTESIAN_POINT('Ctrl Pts',(76.6625281596926,78.8568075952612,210.201113910571));
#28844=CARTESIAN_POINT('Ctrl Pts',(76.8377292359513,78.8141945740678,210.212499998088));
#28845=CARTESIAN_POINT('Ctrl Pts',(76.8377292359507,78.814194574068,210.3));
#28846=CARTESIAN_POINT('Ctrl Pts',(76.7687480941578,78.8309724096837,210.295517006321));
#28847=CARTESIAN_POINT('Ctrl Pts',(76.7008236983214,78.8523550273851,210.290857899815));
#28848=CARTESIAN_POINT('Ctrl Pts',(76.4422757112119,78.9532092563482,210.272143473695));
#28849=CARTESIAN_POINT('Ctrl Pts',(76.2664718582602,79.0645855604091,210.257263400465));
#28850=CARTESIAN_POINT('Ctrl Pts',(75.9609319759317,79.3534488295603,210.22660435113));
#28851=CARTESIAN_POINT('Ctrl Pts',(75.8363263466194,79.5305113967565,210.211117333421));
#28852=CARTESIAN_POINT('Ctrl Pts',(75.6687566621022,79.9130536754183,210.183018492143));
#28853=CARTESIAN_POINT('Ctrl Pts',(75.6234275719121,80.1130022581412,210.17057036958));
#28854=CARTESIAN_POINT('Ctrl Pts',(75.609857319051,80.5247069416304,210.141634497977));
#28855=CARTESIAN_POINT('Ctrl Pts',(75.6438450221561,80.7325813993198,210.126320669189));
#28856=CARTESIAN_POINT('Ctrl Pts',(75.790905719824,81.1268328673936,210.095853279948));
#28857=CARTESIAN_POINT('Ctrl Pts',(75.9038756447547,81.3089509307157,210.081003246673));
#28858=CARTESIAN_POINT('Ctrl Pts',(76.1881755710675,81.6119071707128,210.054639227763));
#28859=CARTESIAN_POINT('Ctrl Pts',(76.3542612929968,81.7323315479678,210.040670851305));
#28860=CARTESIAN_POINT('Ctrl Pts',(76.7298647110601,81.9078268056968,210.010790002062));
#28861=CARTESIAN_POINT('Ctrl Pts',(76.9369831120127,81.9584662165145,209.995258667715));
#28862=CARTESIAN_POINT('Ctrl Pts',(77.3564813822758,81.9762860006598,209.965538873194));
#28863=CARTESIAN_POINT('Ctrl Pts',(77.5646496144558,81.9442707452982,209.952591351819));
#28864=CARTESIAN_POINT('Ctrl Pts',(77.9542715115944,81.8031223657582,209.92493496972));
#28865=CARTESIAN_POINT('Ctrl Pts',(78.1323448530387,81.6964065582324,209.910169851419));
#28866=CARTESIAN_POINT('Ctrl Pts',(78.4443042338802,81.4160685686061,209.879601464765));
#28867=CARTESIAN_POINT('Ctrl Pts',(78.5730919626864,81.2427419612856,209.864081976157));
#28868=CARTESIAN_POINT('Ctrl Pts',(78.7506546572598,80.864784412002,209.83568691703));
#28869=CARTESIAN_POINT('Ctrl Pts',(78.8012631036944,80.665567090636,209.823341973441));
#28870=CARTESIAN_POINT('Ctrl Pts',(78.8252751596618,80.2543567708347,209.794621067973));
#28871=CARTESIAN_POINT('Ctrl Pts',(78.7967470803763,80.0462100137167,209.77938203026));
#28872=CARTESIAN_POINT('Ctrl Pts',(78.6602850281205,79.6486789352933,209.748864919813));
#28873=CARTESIAN_POINT('Ctrl Pts',(78.5521231839478,79.4636145846229,209.733888994856));
#28874=CARTESIAN_POINT('Ctrl Pts',(78.2760699131448,79.1535040912048,209.707160201061));
#28875=CARTESIAN_POINT('Ctrl Pts',(78.1135476494756,79.0289500624745,209.693678439137));
#28876=CARTESIAN_POINT('Ctrl Pts',(77.7436748553578,78.8438260633372,209.664001186349));
#28877=CARTESIAN_POINT('Ctrl Pts',(77.5385938536597,78.787670353911,209.648499326236));
#28878=CARTESIAN_POINT('Ctrl Pts',(77.1634696062218,78.7611896362101,209.62170704795));
#28879=CARTESIAN_POINT('Ctrl Pts',(76.9979584166627,78.7752230699009,209.610413083717));
#28880=CARTESIAN_POINT('Ctrl Pts',(76.8377292359503,78.814194574068,209.6));
#28881=CARTESIAN_POINT('Origin',(77.215862801455,80.368869783441,212.));
#28882=CARTESIAN_POINT('',(76.8377292359511,78.8141945740678,211.));
#28883=CARTESIAN_POINT('',(76.8377292359511,78.8141945740679,210.912499998088));
#28884=CARTESIAN_POINT('',(76.8377292359511,78.8141945740678,212.));
#28885=CARTESIAN_POINT('',(75.7705853637063,79.6824492651474,211.6));
#28886=CARTESIAN_POINT('Ctrl Pts',(75.7705853637062,79.6824492651474,211.6));
#28887=CARTESIAN_POINT('Ctrl Pts',(75.7127116257352,79.8043040254562,211.590812272922));
#28888=CARTESIAN_POINT('Ctrl Pts',(75.6705039153542,79.9329159682097,211.582518428267));
#28889=CARTESIAN_POINT('Ctrl Pts',(75.6185721019073,80.2016904192254,211.564370389863));
#28890=CARTESIAN_POINT('Ctrl Pts',(75.6100956975266,80.3408694116708,211.554655478317));
#28891=CARTESIAN_POINT('Ctrl Pts',(75.6342384712736,80.6896390858489,211.529528724962));
#28892=CARTESIAN_POINT('Ctrl Pts',(75.6902046363061,80.8949879995436,211.514015086573));
#28893=CARTESIAN_POINT('Ctrl Pts',(75.8780514037409,81.2712273915844,211.484121020397));
#28894=CARTESIAN_POINT('Ctrl Pts',(76.0076743264714,81.4385618794624,211.470946087786));
#28895=CARTESIAN_POINT('Ctrl Pts',(76.3208716620126,81.7109516499105,211.443445618933));
#28896=CARTESIAN_POINT('Ctrl Pts',(76.5003440872578,81.8146183718967,211.428761669952));
#28897=CARTESIAN_POINT('Ctrl Pts',(76.8962010668449,81.9510687922483,211.398264057233));
#28898=CARTESIAN_POINT('Ctrl Pts',(77.1098653081239,81.9795617872084,211.382728714258));
#28899=CARTESIAN_POINT('Ctrl Pts',(77.5265895643817,81.9516354056831,211.354140902766));
#28900=CARTESIAN_POINT('Ctrl Pts',(77.7257830195731,81.8991254680589,211.34181973093));
#28901=CARTESIAN_POINT('Ctrl Pts',(78.0970222399127,81.7204382190393,211.313242835828));
#28902=CARTESIAN_POINT('Ctrl Pts',(78.2648981435312,81.5947100816425,211.298058295601));
#28903=CARTESIAN_POINT('Ctrl Pts',(78.5461709019992,81.2828296812592,211.267520255385));
#28904=CARTESIAN_POINT('Ctrl Pts',(78.6555763416884,81.0984676551874,211.252467410117));
#28905=CARTESIAN_POINT('Ctrl Pts',(78.792871469451,80.7067357179128,211.225502630768));
#28906=CARTESIAN_POINT('Ctrl Pts',(78.8229751441819,80.5043436329824,211.212293272722));
#28907=CARTESIAN_POINT('Ctrl Pts',(78.8056160690616,80.0916075495711,211.182751331048));
#28908=CARTESIAN_POINT('Ctrl Pts',(78.7554772361788,79.8853646939831,211.16727477628));
#28909=CARTESIAN_POINT('Ctrl Pts',(78.5778002403132,79.5029311632517,211.137117100773));
#28910=CARTESIAN_POINT('Ctrl Pts',(78.4515978885323,79.3307766817871,211.123521497342));
#28911=CARTESIAN_POINT('Ctrl Pts',(78.1444020505696,79.0498548169265,211.096266062422));
#28912=CARTESIAN_POINT('Ctrl Pts',(77.9680662780484,78.9419376196915,211.081714459557));
#28913=CARTESIAN_POINT('Ctrl Pts',(77.5768771091062,78.7956668446035,211.051342144373));
#28914=CARTESIAN_POINT('Ctrl Pts',(77.3646134045188,78.7616379285038,211.035791308777));
#28915=CARTESIAN_POINT('Ctrl Pts',(77.0457190880988,78.7743972129179,211.013738213079));
#28916=CARTESIAN_POINT('Ctrl Pts',(76.9405061401058,78.7891968144167,211.006679335826));
#28917=CARTESIAN_POINT('Ctrl Pts',(76.8377292359511,78.8141945740678,211.));
#28918=CARTESIAN_POINT('',(76.6545412773313,78.870564692161,211.6));
#28919=CARTESIAN_POINT('Origin',(77.215862801455,80.368869783441,211.6));
#28920=CARTESIAN_POINT('Ctrl Pts',(76.8377292359511,78.8141945740678,210.912499998088));
#28921=CARTESIAN_POINT('Ctrl Pts',(77.038449004072,78.7653748070007,210.925544511827));
#28922=CARTESIAN_POINT('Ctrl Pts',(77.2468954172806,78.7558454971608,210.939935217219));
#28923=CARTESIAN_POINT('Ctrl Pts',(77.6582733012602,78.8171103436994,210.969977480965));
#28924=CARTESIAN_POINT('Ctrl Pts',(77.8569914622933,78.888110439331,210.985338434372));
#28925=CARTESIAN_POINT('Ctrl Pts',(78.210731531279,79.0994384791586,211.014424022625));
#28926=CARTESIAN_POINT('Ctrl Pts',(78.3635562622254,79.2357322791863,211.02699377697));
#28927=CARTESIAN_POINT('Ctrl Pts',(78.6158715202084,79.565695767531,211.054720108117));
#28928=CARTESIAN_POINT('Ctrl Pts',(78.7099829658183,79.7583937882494,211.069994761277));
#28929=CARTESIAN_POINT('Ctrl Pts',(78.8160411588355,80.1636563271765,211.100535715031));
#28930=CARTESIAN_POINT('Ctrl Pts',(78.8291522320142,80.3718099484641,211.115509563216));
#28931=CARTESIAN_POINT('Ctrl Pts',(78.7755087713307,80.7812380709433,211.143593570462));
#28932=CARTESIAN_POINT('Ctrl Pts',(78.7094458670987,80.9785902039949,211.156090429798));
#28933=CARTESIAN_POINT('Ctrl Pts',(78.503038382884,81.3426317847808,211.18530617422));
#28934=CARTESIAN_POINT('Ctrl Pts',(78.3626937012489,81.5045615368933,211.200861380132));
#28935=CARTESIAN_POINT('Ctrl Pts',(78.0333708446082,81.7593284959067,211.231058072714));
#28936=CARTESIAN_POINT('Ctrl Pts',(77.8493872576715,81.8522394178766,211.245439843767));
#28937=CARTESIAN_POINT('Ctrl Pts',(77.4473115727342,81.9663943425186,211.272393964221));
#28938=CARTESIAN_POINT('Ctrl Pts',(77.2320777590094,81.9830148099074,211.286606083563));
#28939=CARTESIAN_POINT('Ctrl Pts',(76.8119112771593,81.9311502697992,211.317070609277));
#28940=CARTESIAN_POINT('Ctrl Pts',(76.6110183595505,81.8648865131105,211.332486638964));
#28941=CARTESIAN_POINT('Ctrl Pts',(76.2520089838787,81.6619802240671,211.361768288196));
#28942=CARTESIAN_POINT('Ctrl Pts',(76.0960651164363,81.5295470033163,211.374561840147));
#28943=CARTESIAN_POINT('Ctrl Pts',(75.8359058962999,81.2060211670675,211.401967228916));
#28944=CARTESIAN_POINT('Ctrl Pts',(75.7371248802881,81.0157058464226,211.417153534263));
#28945=CARTESIAN_POINT('Ctrl Pts',(75.6210516696081,80.6127206269661,211.447705722754));
#28946=CARTESIAN_POINT('Ctrl Pts',(75.6029013253923,80.4044450639927,211.462775050631));
#28947=CARTESIAN_POINT('Ctrl Pts',(75.6468224760359,79.9943725896507,211.491072252065));
#28948=CARTESIAN_POINT('Ctrl Pts',(75.7077324777136,79.7964358226992,211.503445817942));
#28949=CARTESIAN_POINT('Ctrl Pts',(75.8956950985807,79.4443531646425,211.531086608675));
#28950=CARTESIAN_POINT('Ctrl Pts',(76.0172905095577,79.2913820444512,211.545201868697));
#28951=CARTESIAN_POINT('Ctrl Pts',(76.3080221565354,79.0374102574885,211.573323127396));
#28952=CARTESIAN_POINT('Ctrl Pts',(76.4744428920774,78.9380363310756,211.587103998264));
#28953=CARTESIAN_POINT('Ctrl Pts',(76.6545412773326,78.8705646921605,211.6));
#28954=CARTESIAN_POINT('Origin',(77.2158628014545,80.368869783439,198.006249999044));
#28955=CARTESIAN_POINT('',(77.5939963669566,81.9235449928104,211.6));
#28956=CARTESIAN_POINT('',(77.5939963669582,81.9235449928142,211.962499998088));
#28957=CARTESIAN_POINT('',(77.5939963669579,81.9235449928101,198.006249999044));
#28958=CARTESIAN_POINT('Origin',(77.215862801455,80.368869783441,211.6));
#28959=CARTESIAN_POINT('',(76.8377292359511,78.8141945740679,211.7));
#28960=CARTESIAN_POINT('Origin',(77.2158628014592,80.3688697834461,211.641666666667));
#28961=CARTESIAN_POINT('',(76.8377292359511,78.8141945740678,212.312499998088));
#28962=CARTESIAN_POINT('',(76.8377292359511,78.8141945740678,212.006249999044));
#28963=CARTESIAN_POINT('Ctrl Pts',(77.5939963669588,81.9235449928141,211.962499998088));
#28964=CARTESIAN_POINT('Ctrl Pts',(76.6964042163248,82.1418605086474,212.020833331422));
#28965=CARTESIAN_POINT('Ctrl Pts',(76.0585413582559,81.4736806618775,212.079166664755));
#28966=CARTESIAN_POINT('Ctrl Pts',(75.420678500187,80.8055008151075,212.137499998088));
#28967=CARTESIAN_POINT('Ctrl Pts',(75.680407792752,79.9190054525043,212.195833331422));
#28968=CARTESIAN_POINT('Ctrl Pts',(75.9401370853171,79.0325100899011,212.254166664755));
#28969=CARTESIAN_POINT('Ctrl Pts',(76.8377292359511,78.8141945740678,212.312499998088));
#28970=CARTESIAN_POINT('Origin',(77.2158628014549,80.3688697834408,198.006249999044));
#28971=CARTESIAN_POINT('',(77.5044528940591,81.5553919638894,211.568749999044));
#28972=CARTESIAN_POINT('',(77.5044528940591,81.5553919638894,211.743749999044));
#28973=CARTESIAN_POINT('',(77.504452894059,81.555391963889,198.006249999044));
#28974=CARTESIAN_POINT('',(76.9272727088508,79.1823476029925,212.093749999044));
#28975=CARTESIAN_POINT('Ctrl Pts',(77.5044528940591,81.5553919638894,211.743749999044));
#28976=CARTESIAN_POINT('Ctrl Pts',(76.8194139937778,81.7220095315399,211.802083332377));
#28977=CARTESIAN_POINT('Ctrl Pts',(76.332599497335,81.2120572251409,211.860416665711));
#28978=CARTESIAN_POINT('Ctrl Pts',(75.8457850008923,80.7021049187419,211.918749999044));
#28979=CARTESIAN_POINT('Ctrl Pts',(76.0440094047309,80.0255350446925,211.977083332377));
#28980=CARTESIAN_POINT('Ctrl Pts',(76.2422338085695,79.348965170643,212.035416665711));
#28981=CARTESIAN_POINT('Ctrl Pts',(76.9272727088508,79.1823476029925,212.093749999044));
#28982=CARTESIAN_POINT('',(76.9272727088508,79.1823476029925,211.918749999044));
#28983=CARTESIAN_POINT('',(76.9272727088508,79.1823476029925,212.006249999044));
#28984=CARTESIAN_POINT('Ctrl Pts',(77.5044528940591,81.5553919638894,211.568749999044));
#28985=CARTESIAN_POINT('Ctrl Pts',(76.8194139937778,81.7220095315399,211.627083332377));
#28986=CARTESIAN_POINT('Ctrl Pts',(76.332599497335,81.2120572251409,211.685416665711));
#28987=CARTESIAN_POINT('Ctrl Pts',(75.8457850008923,80.7021049187419,211.743749999044));
#28988=CARTESIAN_POINT('Ctrl Pts',(76.0440094047309,80.0255350446925,211.802083332377));
#28989=CARTESIAN_POINT('Ctrl Pts',(76.2422338085695,79.348965170643,211.860416665711));
#28990=CARTESIAN_POINT('Ctrl Pts',(76.9272727088508,79.1823476029925,211.918749999044));
#28991=CARTESIAN_POINT('Origin',(77.2158628014549,80.3688697834408,198.006249999044));
#28992=CARTESIAN_POINT('',(77.5044528940591,81.5553919638894,210.868749999044));
#28993=CARTESIAN_POINT('',(77.5044528940591,81.5553919638894,211.043749999044));
#28994=CARTESIAN_POINT('',(77.504452894059,81.555391963889,198.006249999044));
#28995=CARTESIAN_POINT('Ctrl Pts',(77.5044528940591,81.5553919638894,211.043749999044));
#28996=CARTESIAN_POINT('Ctrl Pts',(76.8194139937778,81.7220095315399,211.102083332377));
#28997=CARTESIAN_POINT('Ctrl Pts',(76.332599497335,81.2120572251409,211.160416665711));
#28998=CARTESIAN_POINT('Ctrl Pts',(75.8457850008923,80.7021049187419,211.218749999044));
#28999=CARTESIAN_POINT('Ctrl Pts',(76.0440094047309,80.0255350446925,211.277083332377));
#29000=CARTESIAN_POINT('Ctrl Pts',(76.2422338085695,79.348965170643,211.335416665711));
#29001=CARTESIAN_POINT('Ctrl Pts',(76.9272727088508,79.1823476029925,211.393749999044));
#29002=CARTESIAN_POINT('Ctrl Pts',(77.6123116091322,79.0157300353421,211.452083332377));
#29003=CARTESIAN_POINT('Ctrl Pts',(78.0991261055749,79.525682341741,211.510416665711));
#29004=CARTESIAN_POINT('Ctrl Pts',(78.5859406020177,80.03563464814,211.568749999044));
#29005=CARTESIAN_POINT('Ctrl Pts',(78.3877161981791,80.7122045221895,211.627083332377));
#29006=CARTESIAN_POINT('Ctrl Pts',(78.1894917943405,81.3887743962389,211.685416665711));
#29007=CARTESIAN_POINT('Ctrl Pts',(77.5044528940591,81.5553919638894,211.743749999044));
#29008=CARTESIAN_POINT('Ctrl Pts',(77.5044528940591,81.5553919638894,210.868749999044));
#29009=CARTESIAN_POINT('Ctrl Pts',(76.8194139937778,81.7220095315399,210.927083332377));
#29010=CARTESIAN_POINT('Ctrl Pts',(76.332599497335,81.2120572251409,210.985416665711));
#29011=CARTESIAN_POINT('Ctrl Pts',(75.8457850008923,80.7021049187419,211.043749999044));
#29012=CARTESIAN_POINT('Ctrl Pts',(76.0440094047309,80.0255350446925,211.102083332377));
#29013=CARTESIAN_POINT('Ctrl Pts',(76.2422338085695,79.348965170643,211.160416665711));
#29014=CARTESIAN_POINT('Ctrl Pts',(76.9272727088508,79.1823476029925,211.218749999044));
#29015=CARTESIAN_POINT('Ctrl Pts',(77.6123116091322,79.0157300353421,211.277083332377));
#29016=CARTESIAN_POINT('Ctrl Pts',(78.0991261055749,79.5256823417411,211.335416665711));
#29017=CARTESIAN_POINT('Ctrl Pts',(78.5859406020177,80.03563464814,211.393749999044));
#29018=CARTESIAN_POINT('Ctrl Pts',(78.3877161981791,80.7122045221895,211.452083332377));
#29019=CARTESIAN_POINT('Ctrl Pts',(78.1894917943405,81.3887743962389,211.510416665711));
#29020=CARTESIAN_POINT('Ctrl Pts',(77.5044528940591,81.5553919638894,211.568749999044));
#29021=CARTESIAN_POINT('Origin',(77.2158628014549,80.3688697834408,198.006249999044));
#29022=CARTESIAN_POINT('',(77.5044528940591,81.5553919638894,210.168749999044));
#29023=CARTESIAN_POINT('',(77.5044528940591,81.5553919638894,210.343749999044));
#29024=CARTESIAN_POINT('',(77.504452894059,81.555391963889,198.006249999044));
#29025=CARTESIAN_POINT('Ctrl Pts',(77.5044528940591,81.5553919638894,210.343749999044));
#29026=CARTESIAN_POINT('Ctrl Pts',(76.8194139937778,81.7220095315399,210.402083332377));
#29027=CARTESIAN_POINT('Ctrl Pts',(76.332599497335,81.2120572251409,210.460416665711));
#29028=CARTESIAN_POINT('Ctrl Pts',(75.8457850008923,80.7021049187419,210.518749999044));
#29029=CARTESIAN_POINT('Ctrl Pts',(76.0440094047309,80.0255350446925,210.577083332377));
#29030=CARTESIAN_POINT('Ctrl Pts',(76.2422338085695,79.348965170643,210.635416665711));
#29031=CARTESIAN_POINT('Ctrl Pts',(76.9272727088508,79.1823476029926,210.693749999044));
#29032=CARTESIAN_POINT('Ctrl Pts',(77.6123116091322,79.0157300353421,210.752083332377));
#29033=CARTESIAN_POINT('Ctrl Pts',(78.0991261055749,79.5256823417411,210.810416665711));
#29034=CARTESIAN_POINT('Ctrl Pts',(78.5859406020177,80.03563464814,210.868749999044));
#29035=CARTESIAN_POINT('Ctrl Pts',(78.3877161981791,80.7122045221895,210.927083332377));
#29036=CARTESIAN_POINT('Ctrl Pts',(78.1894917943405,81.3887743962389,210.985416665711));
#29037=CARTESIAN_POINT('Ctrl Pts',(77.5044528940591,81.5553919638894,211.043749999044));
#29038=CARTESIAN_POINT('Ctrl Pts',(77.5044528940591,81.5553919638894,210.168749999044));
#29039=CARTESIAN_POINT('Ctrl Pts',(76.8194139937778,81.7220095315399,210.227083332377));
#29040=CARTESIAN_POINT('Ctrl Pts',(76.332599497335,81.2120572251409,210.285416665711));
#29041=CARTESIAN_POINT('Ctrl Pts',(75.8457850008923,80.7021049187419,210.343749999044));
#29042=CARTESIAN_POINT('Ctrl Pts',(76.0440094047309,80.0255350446925,210.402083332377));
#29043=CARTESIAN_POINT('Ctrl Pts',(76.2422338085695,79.348965170643,210.460416665711));
#29044=CARTESIAN_POINT('Ctrl Pts',(76.9272727088508,79.1823476029926,210.518749999044));
#29045=CARTESIAN_POINT('Ctrl Pts',(77.6123116091322,79.0157300353421,210.577083332377));
#29046=CARTESIAN_POINT('Ctrl Pts',(78.0991261055749,79.5256823417411,210.635416665711));
#29047=CARTESIAN_POINT('Ctrl Pts',(78.5859406020177,80.03563464814,210.693749999044));
#29048=CARTESIAN_POINT('Ctrl Pts',(78.3877161981791,80.7122045221895,210.752083332377));
#29049=CARTESIAN_POINT('Ctrl Pts',(78.1894917943405,81.3887743962389,210.810416665711));
#29050=CARTESIAN_POINT('Ctrl Pts',(77.5044528940591,81.5553919638894,210.868749999044));
#29051=CARTESIAN_POINT('Origin',(77.2158628014549,80.3688697834408,198.006249999044));
#29052=CARTESIAN_POINT('',(77.5044528940591,81.5553919638894,209.468749999044));
#29053=CARTESIAN_POINT('',(77.5044528940591,81.5553919638894,209.643749999044));
#29054=CARTESIAN_POINT('',(77.504452894059,81.555391963889,198.006249999044));
#29055=CARTESIAN_POINT('Ctrl Pts',(77.5044528940591,81.5553919638894,209.643749999044));
#29056=CARTESIAN_POINT('Ctrl Pts',(76.8194139937778,81.7220095315399,209.702083332377));
#29057=CARTESIAN_POINT('Ctrl Pts',(76.332599497335,81.2120572251409,209.760416665711));
#29058=CARTESIAN_POINT('Ctrl Pts',(75.8457850008923,80.7021049187419,209.818749999044));
#29059=CARTESIAN_POINT('Ctrl Pts',(76.0440094047309,80.0255350446925,209.877083332377));
#29060=CARTESIAN_POINT('Ctrl Pts',(76.2422338085695,79.348965170643,209.935416665711));
#29061=CARTESIAN_POINT('Ctrl Pts',(76.9272727088508,79.1823476029926,209.993749999044));
#29062=CARTESIAN_POINT('Ctrl Pts',(77.6123116091322,79.0157300353421,210.052083332377));
#29063=CARTESIAN_POINT('Ctrl Pts',(78.0991261055749,79.5256823417411,210.110416665711));
#29064=CARTESIAN_POINT('Ctrl Pts',(78.5859406020177,80.03563464814,210.168749999044));
#29065=CARTESIAN_POINT('Ctrl Pts',(78.3877161981791,80.7122045221895,210.227083332377));
#29066=CARTESIAN_POINT('Ctrl Pts',(78.1894917943405,81.3887743962389,210.285416665711));
#29067=CARTESIAN_POINT('Ctrl Pts',(77.5044528940591,81.5553919638894,210.343749999044));
#29068=CARTESIAN_POINT('Ctrl Pts',(77.5044528940591,81.5553919638894,209.468749999044));
#29069=CARTESIAN_POINT('Ctrl Pts',(76.8194139937778,81.7220095315399,209.527083332377));
#29070=CARTESIAN_POINT('Ctrl Pts',(76.332599497335,81.2120572251409,209.585416665711));
#29071=CARTESIAN_POINT('Ctrl Pts',(75.8457850008923,80.7021049187419,209.643749999044));
#29072=CARTESIAN_POINT('Ctrl Pts',(76.0440094047309,80.0255350446925,209.702083332377));
#29073=CARTESIAN_POINT('Ctrl Pts',(76.2422338085695,79.348965170643,209.760416665711));
#29074=CARTESIAN_POINT('Ctrl Pts',(76.9272727088508,79.1823476029926,209.818749999044));
#29075=CARTESIAN_POINT('Ctrl Pts',(77.6123116091322,79.0157300353421,209.877083332377));
#29076=CARTESIAN_POINT('Ctrl Pts',(78.0991261055749,79.5256823417411,209.935416665711));
#29077=CARTESIAN_POINT('Ctrl Pts',(78.5859406020177,80.03563464814,209.993749999044));
#29078=CARTESIAN_POINT('Ctrl Pts',(78.3877161981791,80.7122045221895,210.052083332377));
#29079=CARTESIAN_POINT('Ctrl Pts',(78.1894917943405,81.3887743962389,210.110416665711));
#29080=CARTESIAN_POINT('Ctrl Pts',(77.5044528940591,81.5553919638894,210.168749999044));
#29081=CARTESIAN_POINT('Origin',(77.2158628014549,80.3688697834408,198.006249999044));
#29082=CARTESIAN_POINT('',(77.5044528940591,81.5553919638894,208.768749999044));
#29083=CARTESIAN_POINT('',(77.5044528940591,81.5553919638894,208.943749999044));
#29084=CARTESIAN_POINT('',(77.504452894059,81.555391963889,198.006249999044));
#29085=CARTESIAN_POINT('Ctrl Pts',(77.5044528940591,81.5553919638894,208.943749999044));
#29086=CARTESIAN_POINT('Ctrl Pts',(76.8194139937778,81.7220095315399,209.002083332377));
#29087=CARTESIAN_POINT('Ctrl Pts',(76.332599497335,81.2120572251409,209.060416665711));
#29088=CARTESIAN_POINT('Ctrl Pts',(75.8457850008923,80.7021049187419,209.118749999044));
#29089=CARTESIAN_POINT('Ctrl Pts',(76.0440094047309,80.0255350446925,209.177083332377));
#29090=CARTESIAN_POINT('Ctrl Pts',(76.2422338085695,79.348965170643,209.235416665711));
#29091=CARTESIAN_POINT('Ctrl Pts',(76.9272727088508,79.1823476029926,209.293749999044));
#29092=CARTESIAN_POINT('Ctrl Pts',(77.6123116091322,79.0157300353421,209.352083332377));
#29093=CARTESIAN_POINT('Ctrl Pts',(78.0991261055749,79.5256823417411,209.410416665711));
#29094=CARTESIAN_POINT('Ctrl Pts',(78.5859406020177,80.03563464814,209.468749999044));
#29095=CARTESIAN_POINT('Ctrl Pts',(78.3877161981791,80.7122045221895,209.527083332377));
#29096=CARTESIAN_POINT('Ctrl Pts',(78.1894917943405,81.3887743962389,209.585416665711));
#29097=CARTESIAN_POINT('Ctrl Pts',(77.5044528940591,81.5553919638894,209.643749999044));
#29098=CARTESIAN_POINT('Ctrl Pts',(77.5044528940591,81.5553919638894,208.768749999044));
#29099=CARTESIAN_POINT('Ctrl Pts',(76.8194139937778,81.7220095315399,208.827083332377));
#29100=CARTESIAN_POINT('Ctrl Pts',(76.332599497335,81.2120572251409,208.885416665711));
#29101=CARTESIAN_POINT('Ctrl Pts',(75.8457850008923,80.7021049187419,208.943749999044));
#29102=CARTESIAN_POINT('Ctrl Pts',(76.0440094047309,80.0255350446925,209.002083332377));
#29103=CARTESIAN_POINT('Ctrl Pts',(76.2422338085695,79.348965170643,209.060416665711));
#29104=CARTESIAN_POINT('Ctrl Pts',(76.9272727088508,79.1823476029926,209.118749999044));
#29105=CARTESIAN_POINT('Ctrl Pts',(77.6123116091322,79.0157300353421,209.177083332377));
#29106=CARTESIAN_POINT('Ctrl Pts',(78.0991261055749,79.5256823417411,209.235416665711));
#29107=CARTESIAN_POINT('Ctrl Pts',(78.5859406020177,80.03563464814,209.293749999044));
#29108=CARTESIAN_POINT('Ctrl Pts',(78.3877161981791,80.7122045221895,209.352083332377));
#29109=CARTESIAN_POINT('Ctrl Pts',(78.1894917943405,81.3887743962389,209.410416665711));
#29110=CARTESIAN_POINT('Ctrl Pts',(77.5044528940591,81.5553919638894,209.468749999044));
#29111=CARTESIAN_POINT('Origin',(77.2158628014549,80.3688697834408,198.006249999044));
#29112=CARTESIAN_POINT('',(77.5044528940591,81.5553919638894,208.068749999044));
#29113=CARTESIAN_POINT('',(77.5044528940591,81.5553919638894,208.243749999044));
#29114=CARTESIAN_POINT('',(77.504452894059,81.555391963889,198.006249999044));
#29115=CARTESIAN_POINT('Ctrl Pts',(77.5044528940591,81.5553919638894,208.243749999044));
#29116=CARTESIAN_POINT('Ctrl Pts',(76.8194139937778,81.7220095315399,208.302083332377));
#29117=CARTESIAN_POINT('Ctrl Pts',(76.332599497335,81.2120572251409,208.360416665711));
#29118=CARTESIAN_POINT('Ctrl Pts',(75.8457850008923,80.7021049187419,208.418749999044));
#29119=CARTESIAN_POINT('Ctrl Pts',(76.0440094047309,80.0255350446925,208.477083332377));
#29120=CARTESIAN_POINT('Ctrl Pts',(76.2422338085695,79.348965170643,208.535416665711));
#29121=CARTESIAN_POINT('Ctrl Pts',(76.9272727088508,79.1823476029926,208.593749999044));
#29122=CARTESIAN_POINT('Ctrl Pts',(77.6123116091322,79.0157300353421,208.652083332377));
#29123=CARTESIAN_POINT('Ctrl Pts',(78.0991261055749,79.5256823417411,208.710416665711));
#29124=CARTESIAN_POINT('Ctrl Pts',(78.5859406020177,80.03563464814,208.768749999044));
#29125=CARTESIAN_POINT('Ctrl Pts',(78.3877161981791,80.7122045221895,208.827083332377));
#29126=CARTESIAN_POINT('Ctrl Pts',(78.1894917943405,81.3887743962389,208.885416665711));
#29127=CARTESIAN_POINT('Ctrl Pts',(77.5044528940591,81.5553919638894,208.943749999044));
#29128=CARTESIAN_POINT('Ctrl Pts',(77.5044528940591,81.5553919638894,208.068749999044));
#29129=CARTESIAN_POINT('Ctrl Pts',(76.8194139937778,81.7220095315399,208.127083332377));
#29130=CARTESIAN_POINT('Ctrl Pts',(76.332599497335,81.2120572251409,208.185416665711));
#29131=CARTESIAN_POINT('Ctrl Pts',(75.8457850008923,80.7021049187419,208.243749999044));
#29132=CARTESIAN_POINT('Ctrl Pts',(76.0440094047309,80.0255350446925,208.302083332377));
#29133=CARTESIAN_POINT('Ctrl Pts',(76.2422338085695,79.348965170643,208.360416665711));
#29134=CARTESIAN_POINT('Ctrl Pts',(76.9272727088508,79.1823476029926,208.418749999044));
#29135=CARTESIAN_POINT('Ctrl Pts',(77.6123116091322,79.0157300353421,208.477083332377));
#29136=CARTESIAN_POINT('Ctrl Pts',(78.0991261055749,79.5256823417411,208.535416665711));
#29137=CARTESIAN_POINT('Ctrl Pts',(78.5859406020177,80.03563464814,208.593749999044));
#29138=CARTESIAN_POINT('Ctrl Pts',(78.3877161981791,80.7122045221895,208.652083332377));
#29139=CARTESIAN_POINT('Ctrl Pts',(78.1894917943405,81.3887743962389,208.710416665711));
#29140=CARTESIAN_POINT('Ctrl Pts',(77.5044528940591,81.5553919638894,208.768749999044));
#29141=CARTESIAN_POINT('Origin',(77.2158628014549,80.3688697834408,198.006249999044));
#29142=CARTESIAN_POINT('',(77.5044528940591,81.5553919638894,207.368749999044));
#29143=CARTESIAN_POINT('',(77.5044528940591,81.5553919638894,207.543749999044));
#29144=CARTESIAN_POINT('',(77.504452894059,81.555391963889,198.006249999044));
#29145=CARTESIAN_POINT('Ctrl Pts',(77.5044528940591,81.5553919638894,207.543749999044));
#29146=CARTESIAN_POINT('Ctrl Pts',(76.8194139937778,81.7220095315399,207.602083332377));
#29147=CARTESIAN_POINT('Ctrl Pts',(76.332599497335,81.2120572251409,207.660416665711));
#29148=CARTESIAN_POINT('Ctrl Pts',(75.8457850008923,80.7021049187419,207.718749999044));
#29149=CARTESIAN_POINT('Ctrl Pts',(76.0440094047309,80.0255350446925,207.777083332377));
#29150=CARTESIAN_POINT('Ctrl Pts',(76.2422338085695,79.348965170643,207.835416665711));
#29151=CARTESIAN_POINT('Ctrl Pts',(76.9272727088508,79.1823476029926,207.893749999044));
#29152=CARTESIAN_POINT('Ctrl Pts',(77.6123116091322,79.0157300353421,207.952083332377));
#29153=CARTESIAN_POINT('Ctrl Pts',(78.0991261055749,79.5256823417411,208.010416665711));
#29154=CARTESIAN_POINT('Ctrl Pts',(78.5859406020177,80.03563464814,208.068749999044));
#29155=CARTESIAN_POINT('Ctrl Pts',(78.3877161981791,80.7122045221895,208.127083332377));
#29156=CARTESIAN_POINT('Ctrl Pts',(78.1894917943405,81.3887743962389,208.185416665711));
#29157=CARTESIAN_POINT('Ctrl Pts',(77.5044528940591,81.5553919638894,208.243749999044));
#29158=CARTESIAN_POINT('Ctrl Pts',(77.5044528940591,81.5553919638894,207.368749999044));
#29159=CARTESIAN_POINT('Ctrl Pts',(76.8194139937778,81.7220095315399,207.427083332377));
#29160=CARTESIAN_POINT('Ctrl Pts',(76.332599497335,81.2120572251409,207.485416665711));
#29161=CARTESIAN_POINT('Ctrl Pts',(75.8457850008923,80.7021049187419,207.543749999044));
#29162=CARTESIAN_POINT('Ctrl Pts',(76.0440094047309,80.0255350446925,207.602083332377));
#29163=CARTESIAN_POINT('Ctrl Pts',(76.2422338085695,79.348965170643,207.660416665711));
#29164=CARTESIAN_POINT('Ctrl Pts',(76.9272727088508,79.1823476029926,207.718749999044));
#29165=CARTESIAN_POINT('Ctrl Pts',(77.6123116091322,79.0157300353421,207.777083332377));
#29166=CARTESIAN_POINT('Ctrl Pts',(78.0991261055749,79.5256823417411,207.835416665711));
#29167=CARTESIAN_POINT('Ctrl Pts',(78.5859406020177,80.03563464814,207.893749999044));
#29168=CARTESIAN_POINT('Ctrl Pts',(78.3877161981791,80.7122045221895,207.952083332377));
#29169=CARTESIAN_POINT('Ctrl Pts',(78.1894917943405,81.3887743962389,208.010416665711));
#29170=CARTESIAN_POINT('Ctrl Pts',(77.5044528940591,81.5553919638894,208.068749999044));
#29171=CARTESIAN_POINT('Origin',(77.2158628014549,80.3688697834408,198.006249999044));
#29172=CARTESIAN_POINT('',(77.5044528940591,81.5553919638894,206.668749999044));
#29173=CARTESIAN_POINT('',(77.5044528940591,81.5553919638894,206.843749999044));
#29174=CARTESIAN_POINT('',(77.504452894059,81.555391963889,198.006249999044));
#29175=CARTESIAN_POINT('Ctrl Pts',(77.5044528940591,81.5553919638894,206.843749999044));
#29176=CARTESIAN_POINT('Ctrl Pts',(76.8194139937778,81.7220095315399,206.902083332377));
#29177=CARTESIAN_POINT('Ctrl Pts',(76.332599497335,81.2120572251409,206.960416665711));
#29178=CARTESIAN_POINT('Ctrl Pts',(75.8457850008923,80.7021049187419,207.018749999044));
#29179=CARTESIAN_POINT('Ctrl Pts',(76.0440094047309,80.0255350446925,207.077083332377));
#29180=CARTESIAN_POINT('Ctrl Pts',(76.2422338085695,79.348965170643,207.135416665711));
#29181=CARTESIAN_POINT('Ctrl Pts',(76.9272727088508,79.1823476029926,207.193749999044));
#29182=CARTESIAN_POINT('Ctrl Pts',(77.6123116091322,79.0157300353421,207.252083332377));
#29183=CARTESIAN_POINT('Ctrl Pts',(78.099126105575,79.5256823417411,207.310416665711));
#29184=CARTESIAN_POINT('Ctrl Pts',(78.5859406020177,80.03563464814,207.368749999044));
#29185=CARTESIAN_POINT('Ctrl Pts',(78.3877161981791,80.7122045221895,207.427083332377));
#29186=CARTESIAN_POINT('Ctrl Pts',(78.1894917943405,81.3887743962389,207.485416665711));
#29187=CARTESIAN_POINT('Ctrl Pts',(77.5044528940591,81.5553919638894,207.543749999044));
#29188=CARTESIAN_POINT('Ctrl Pts',(77.5044528940591,81.5553919638894,206.668749999044));
#29189=CARTESIAN_POINT('Ctrl Pts',(76.8194139937778,81.7220095315399,206.727083332378));
#29190=CARTESIAN_POINT('Ctrl Pts',(76.332599497335,81.2120572251409,206.785416665711));
#29191=CARTESIAN_POINT('Ctrl Pts',(75.8457850008923,80.7021049187419,206.843749999044));
#29192=CARTESIAN_POINT('Ctrl Pts',(76.0440094047309,80.0255350446925,206.902083332377));
#29193=CARTESIAN_POINT('Ctrl Pts',(76.2422338085695,79.348965170643,206.960416665711));
#29194=CARTESIAN_POINT('Ctrl Pts',(76.9272727088508,79.1823476029926,207.018749999044));
#29195=CARTESIAN_POINT('Ctrl Pts',(77.6123116091322,79.0157300353421,207.077083332377));
#29196=CARTESIAN_POINT('Ctrl Pts',(78.099126105575,79.5256823417411,207.135416665711));
#29197=CARTESIAN_POINT('Ctrl Pts',(78.5859406020177,80.03563464814,207.193749999044));
#29198=CARTESIAN_POINT('Ctrl Pts',(78.3877161981791,80.7122045221895,207.252083332377));
#29199=CARTESIAN_POINT('Ctrl Pts',(78.1894917943405,81.3887743962389,207.310416665711));
#29200=CARTESIAN_POINT('Ctrl Pts',(77.5044528940591,81.5553919638894,207.368749999044));
#29201=CARTESIAN_POINT('Origin',(77.2158628014549,80.3688697834408,198.006249999044));
#29202=CARTESIAN_POINT('',(77.5044528940591,81.5553919638894,205.968749999044));
#29203=CARTESIAN_POINT('',(77.5044528940591,81.5553919638894,206.143749999044));
#29204=CARTESIAN_POINT('',(77.504452894059,81.555391963889,198.006249999044));
#29205=CARTESIAN_POINT('Ctrl Pts',(77.5044528940591,81.5553919638894,206.143749999044));
#29206=CARTESIAN_POINT('Ctrl Pts',(76.8194139937778,81.7220095315399,206.202083332377));
#29207=CARTESIAN_POINT('Ctrl Pts',(76.332599497335,81.2120572251409,206.260416665711));
#29208=CARTESIAN_POINT('Ctrl Pts',(75.8457850008923,80.7021049187419,206.318749999044));
#29209=CARTESIAN_POINT('Ctrl Pts',(76.0440094047309,80.0255350446925,206.377083332377));
#29210=CARTESIAN_POINT('Ctrl Pts',(76.2422338085695,79.348965170643,206.435416665711));
#29211=CARTESIAN_POINT('Ctrl Pts',(76.9272727088508,79.1823476029926,206.493749999044));
#29212=CARTESIAN_POINT('Ctrl Pts',(77.6123116091322,79.0157300353421,206.552083332377));
#29213=CARTESIAN_POINT('Ctrl Pts',(78.099126105575,79.5256823417411,206.610416665711));
#29214=CARTESIAN_POINT('Ctrl Pts',(78.5859406020177,80.03563464814,206.668749999044));
#29215=CARTESIAN_POINT('Ctrl Pts',(78.3877161981791,80.7122045221895,206.727083332377));
#29216=CARTESIAN_POINT('Ctrl Pts',(78.1894917943405,81.3887743962389,206.785416665711));
#29217=CARTESIAN_POINT('Ctrl Pts',(77.5044528940591,81.5553919638894,206.843749999044));
#29218=CARTESIAN_POINT('Ctrl Pts',(77.5044528940591,81.5553919638894,205.968749999044));
#29219=CARTESIAN_POINT('Ctrl Pts',(76.8194139937778,81.7220095315399,206.027083332377));
#29220=CARTESIAN_POINT('Ctrl Pts',(76.332599497335,81.2120572251409,206.085416665711));
#29221=CARTESIAN_POINT('Ctrl Pts',(75.8457850008923,80.7021049187419,206.143749999044));
#29222=CARTESIAN_POINT('Ctrl Pts',(76.0440094047309,80.0255350446925,206.202083332377));
#29223=CARTESIAN_POINT('Ctrl Pts',(76.2422338085695,79.348965170643,206.260416665711));
#29224=CARTESIAN_POINT('Ctrl Pts',(76.9272727088508,79.1823476029926,206.318749999044));
#29225=CARTESIAN_POINT('Ctrl Pts',(77.6123116091322,79.0157300353421,206.377083332377));
#29226=CARTESIAN_POINT('Ctrl Pts',(78.099126105575,79.5256823417411,206.435416665711));
#29227=CARTESIAN_POINT('Ctrl Pts',(78.5859406020177,80.03563464814,206.493749999044));
#29228=CARTESIAN_POINT('Ctrl Pts',(78.3877161981791,80.7122045221895,206.552083332377));
#29229=CARTESIAN_POINT('Ctrl Pts',(78.1894917943405,81.3887743962389,206.610416665711));
#29230=CARTESIAN_POINT('Ctrl Pts',(77.5044528940591,81.5553919638894,206.668749999044));
#29231=CARTESIAN_POINT('Origin',(77.2158628014549,80.3688697834408,198.006249999044));
#29232=CARTESIAN_POINT('',(77.5044528940591,81.5553919638894,205.268749999044));
#29233=CARTESIAN_POINT('',(77.5044528940591,81.5553919638894,205.443749999044));
#29234=CARTESIAN_POINT('',(77.504452894059,81.555391963889,198.006249999044));
#29235=CARTESIAN_POINT('Ctrl Pts',(77.5044528940591,81.5553919638894,205.443749999044));
#29236=CARTESIAN_POINT('Ctrl Pts',(76.8194139937778,81.7220095315399,205.502083332377));
#29237=CARTESIAN_POINT('Ctrl Pts',(76.332599497335,81.2120572251409,205.560416665711));
#29238=CARTESIAN_POINT('Ctrl Pts',(75.8457850008923,80.7021049187419,205.618749999044));
#29239=CARTESIAN_POINT('Ctrl Pts',(76.0440094047309,80.0255350446925,205.677083332377));
#29240=CARTESIAN_POINT('Ctrl Pts',(76.2422338085695,79.348965170643,205.735416665711));
#29241=CARTESIAN_POINT('Ctrl Pts',(76.9272727088508,79.1823476029926,205.793749999044));
#29242=CARTESIAN_POINT('Ctrl Pts',(77.6123116091322,79.0157300353421,205.852083332377));
#29243=CARTESIAN_POINT('Ctrl Pts',(78.099126105575,79.5256823417411,205.910416665711));
#29244=CARTESIAN_POINT('Ctrl Pts',(78.5859406020177,80.03563464814,205.968749999044));
#29245=CARTESIAN_POINT('Ctrl Pts',(78.3877161981791,80.7122045221895,206.027083332377));
#29246=CARTESIAN_POINT('Ctrl Pts',(78.1894917943405,81.3887743962389,206.085416665711));
#29247=CARTESIAN_POINT('Ctrl Pts',(77.5044528940591,81.5553919638894,206.143749999044));
#29248=CARTESIAN_POINT('Ctrl Pts',(77.5044528940591,81.5553919638894,205.268749999044));
#29249=CARTESIAN_POINT('Ctrl Pts',(76.8194139937778,81.7220095315399,205.327083332377));
#29250=CARTESIAN_POINT('Ctrl Pts',(76.332599497335,81.2120572251409,205.385416665711));
#29251=CARTESIAN_POINT('Ctrl Pts',(75.8457850008923,80.7021049187419,205.443749999044));
#29252=CARTESIAN_POINT('Ctrl Pts',(76.0440094047309,80.0255350446925,205.502083332377));
#29253=CARTESIAN_POINT('Ctrl Pts',(76.2422338085695,79.348965170643,205.560416665711));
#29254=CARTESIAN_POINT('Ctrl Pts',(76.9272727088508,79.1823476029926,205.618749999044));
#29255=CARTESIAN_POINT('Ctrl Pts',(77.6123116091322,79.0157300353421,205.677083332377));
#29256=CARTESIAN_POINT('Ctrl Pts',(78.099126105575,79.5256823417411,205.735416665711));
#29257=CARTESIAN_POINT('Ctrl Pts',(78.5859406020177,80.03563464814,205.793749999044));
#29258=CARTESIAN_POINT('Ctrl Pts',(78.3877161981791,80.7122045221895,205.852083332377));
#29259=CARTESIAN_POINT('Ctrl Pts',(78.1894917943405,81.388774396239,205.910416665711));
#29260=CARTESIAN_POINT('Ctrl Pts',(77.5044528940591,81.5553919638894,205.968749999044));
#29261=CARTESIAN_POINT('Origin',(77.2158628014549,80.3688697834408,198.006249999044));
#29262=CARTESIAN_POINT('',(77.5044528940591,81.5553919638894,204.568749999044));
#29263=CARTESIAN_POINT('',(77.5044528940591,81.5553919638894,204.743749999044));
#29264=CARTESIAN_POINT('',(77.504452894059,81.555391963889,198.006249999044));
#29265=CARTESIAN_POINT('Ctrl Pts',(77.5044528940591,81.5553919638894,204.743749999044));
#29266=CARTESIAN_POINT('Ctrl Pts',(76.8194139937778,81.7220095315399,204.802083332378));
#29267=CARTESIAN_POINT('Ctrl Pts',(76.332599497335,81.2120572251409,204.860416665711));
#29268=CARTESIAN_POINT('Ctrl Pts',(75.8457850008923,80.7021049187419,204.918749999044));
#29269=CARTESIAN_POINT('Ctrl Pts',(76.0440094047309,80.0255350446925,204.977083332377));
#29270=CARTESIAN_POINT('Ctrl Pts',(76.2422338085695,79.348965170643,205.035416665711));
#29271=CARTESIAN_POINT('Ctrl Pts',(76.9272727088508,79.1823476029926,205.093749999044));
#29272=CARTESIAN_POINT('Ctrl Pts',(77.6123116091322,79.0157300353421,205.152083332377));
#29273=CARTESIAN_POINT('Ctrl Pts',(78.099126105575,79.5256823417411,205.210416665711));
#29274=CARTESIAN_POINT('Ctrl Pts',(78.5859406020177,80.03563464814,205.268749999044));
#29275=CARTESIAN_POINT('Ctrl Pts',(78.3877161981791,80.7122045221895,205.327083332377));
#29276=CARTESIAN_POINT('Ctrl Pts',(78.1894917943405,81.388774396239,205.385416665711));
#29277=CARTESIAN_POINT('Ctrl Pts',(77.5044528940591,81.5553919638894,205.443749999044));
#29278=CARTESIAN_POINT('Ctrl Pts',(77.5044528940591,81.5553919638894,204.568749999044));
#29279=CARTESIAN_POINT('Ctrl Pts',(76.8194139937778,81.7220095315399,204.627083332377));
#29280=CARTESIAN_POINT('Ctrl Pts',(76.332599497335,81.2120572251409,204.685416665711));
#29281=CARTESIAN_POINT('Ctrl Pts',(75.8457850008923,80.7021049187419,204.743749999044));
#29282=CARTESIAN_POINT('Ctrl Pts',(76.0440094047309,80.0255350446925,204.802083332377));
#29283=CARTESIAN_POINT('Ctrl Pts',(76.2422338085695,79.348965170643,204.860416665711));
#29284=CARTESIAN_POINT('Ctrl Pts',(76.9272727088508,79.1823476029926,204.918749999044));
#29285=CARTESIAN_POINT('Ctrl Pts',(77.6123116091322,79.0157300353421,204.977083332377));
#29286=CARTESIAN_POINT('Ctrl Pts',(78.099126105575,79.5256823417411,205.035416665711));
#29287=CARTESIAN_POINT('Ctrl Pts',(78.5859406020177,80.03563464814,205.093749999044));
#29288=CARTESIAN_POINT('Ctrl Pts',(78.3877161981791,80.7122045221895,205.152083332377));
#29289=CARTESIAN_POINT('Ctrl Pts',(78.1894917943405,81.388774396239,205.210416665711));
#29290=CARTESIAN_POINT('Ctrl Pts',(77.5044528940591,81.5553919638894,205.268749999044));
#29291=CARTESIAN_POINT('Origin',(77.2158628014549,80.3688697834408,198.006249999044));
#29292=CARTESIAN_POINT('',(77.5044528940591,81.5553919638894,203.868749999044));
#29293=CARTESIAN_POINT('',(77.5044528940591,81.5553919638894,204.043749999044));
#29294=CARTESIAN_POINT('',(77.504452894059,81.555391963889,198.006249999044));
#29295=CARTESIAN_POINT('Ctrl Pts',(77.5044528940591,81.5553919638894,204.043749999044));
#29296=CARTESIAN_POINT('Ctrl Pts',(76.8194139937778,81.7220095315399,204.102083332377));
#29297=CARTESIAN_POINT('Ctrl Pts',(76.332599497335,81.2120572251409,204.160416665711));
#29298=CARTESIAN_POINT('Ctrl Pts',(75.8457850008923,80.7021049187419,204.218749999044));
#29299=CARTESIAN_POINT('Ctrl Pts',(76.0440094047309,80.0255350446925,204.277083332377));
#29300=CARTESIAN_POINT('Ctrl Pts',(76.2422338085695,79.348965170643,204.335416665711));
#29301=CARTESIAN_POINT('Ctrl Pts',(76.9272727088508,79.1823476029926,204.393749999044));
#29302=CARTESIAN_POINT('Ctrl Pts',(77.6123116091322,79.0157300353421,204.452083332377));
#29303=CARTESIAN_POINT('Ctrl Pts',(78.099126105575,79.5256823417411,204.510416665711));
#29304=CARTESIAN_POINT('Ctrl Pts',(78.5859406020177,80.03563464814,204.568749999044));
#29305=CARTESIAN_POINT('Ctrl Pts',(78.3877161981791,80.7122045221895,204.627083332377));
#29306=CARTESIAN_POINT('Ctrl Pts',(78.1894917943405,81.388774396239,204.685416665711));
#29307=CARTESIAN_POINT('Ctrl Pts',(77.5044528940591,81.5553919638894,204.743749999044));
#29308=CARTESIAN_POINT('Ctrl Pts',(77.5044528940591,81.5553919638894,203.868749999044));
#29309=CARTESIAN_POINT('Ctrl Pts',(76.8194139937778,81.7220095315399,203.927083332377));
#29310=CARTESIAN_POINT('Ctrl Pts',(76.332599497335,81.2120572251409,203.985416665711));
#29311=CARTESIAN_POINT('Ctrl Pts',(75.8457850008923,80.7021049187419,204.043749999044));
#29312=CARTESIAN_POINT('Ctrl Pts',(76.0440094047309,80.0255350446925,204.102083332377));
#29313=CARTESIAN_POINT('Ctrl Pts',(76.2422338085695,79.348965170643,204.160416665711));
#29314=CARTESIAN_POINT('Ctrl Pts',(76.9272727088508,79.1823476029926,204.218749999044));
#29315=CARTESIAN_POINT('Ctrl Pts',(77.6123116091322,79.0157300353421,204.277083332377));
#29316=CARTESIAN_POINT('Ctrl Pts',(78.099126105575,79.5256823417411,204.335416665711));
#29317=CARTESIAN_POINT('Ctrl Pts',(78.5859406020177,80.03563464814,204.393749999044));
#29318=CARTESIAN_POINT('Ctrl Pts',(78.3877161981791,80.7122045221895,204.452083332377));
#29319=CARTESIAN_POINT('Ctrl Pts',(78.1894917943405,81.388774396239,204.510416665711));
#29320=CARTESIAN_POINT('Ctrl Pts',(77.5044528940591,81.5553919638894,204.568749999044));
#29321=CARTESIAN_POINT('Origin',(77.2158628014549,80.3688697834408,198.006249999044));
#29322=CARTESIAN_POINT('',(77.5044528940591,81.5553919638894,203.168749999044));
#29323=CARTESIAN_POINT('',(77.5044528940591,81.5553919638894,203.343749999044));
#29324=CARTESIAN_POINT('',(77.504452894059,81.555391963889,198.006249999044));
#29325=CARTESIAN_POINT('Ctrl Pts',(77.5044528940591,81.5553919638894,203.343749999044));
#29326=CARTESIAN_POINT('Ctrl Pts',(76.8194139937778,81.7220095315399,203.402083332378));
#29327=CARTESIAN_POINT('Ctrl Pts',(76.332599497335,81.2120572251409,203.460416665711));
#29328=CARTESIAN_POINT('Ctrl Pts',(75.8457850008923,80.7021049187419,203.518749999044));
#29329=CARTESIAN_POINT('Ctrl Pts',(76.0440094047309,80.0255350446925,203.577083332377));
#29330=CARTESIAN_POINT('Ctrl Pts',(76.2422338085695,79.348965170643,203.635416665711));
#29331=CARTESIAN_POINT('Ctrl Pts',(76.9272727088508,79.1823476029926,203.693749999044));
#29332=CARTESIAN_POINT('Ctrl Pts',(77.6123116091322,79.0157300353421,203.752083332377));
#29333=CARTESIAN_POINT('Ctrl Pts',(78.099126105575,79.5256823417411,203.810416665711));
#29334=CARTESIAN_POINT('Ctrl Pts',(78.5859406020177,80.03563464814,203.868749999044));
#29335=CARTESIAN_POINT('Ctrl Pts',(78.3877161981791,80.7122045221895,203.927083332377));
#29336=CARTESIAN_POINT('Ctrl Pts',(78.1894917943405,81.388774396239,203.985416665711));
#29337=CARTESIAN_POINT('Ctrl Pts',(77.5044528940591,81.5553919638894,204.043749999044));
#29338=CARTESIAN_POINT('Ctrl Pts',(77.5044528940591,81.5553919638894,203.168749999044));
#29339=CARTESIAN_POINT('Ctrl Pts',(76.8194139937778,81.7220095315399,203.227083332378));
#29340=CARTESIAN_POINT('Ctrl Pts',(76.332599497335,81.2120572251409,203.285416665711));
#29341=CARTESIAN_POINT('Ctrl Pts',(75.8457850008923,80.7021049187419,203.343749999044));
#29342=CARTESIAN_POINT('Ctrl Pts',(76.0440094047309,80.0255350446925,203.402083332377));
#29343=CARTESIAN_POINT('Ctrl Pts',(76.2422338085695,79.348965170643,203.460416665711));
#29344=CARTESIAN_POINT('Ctrl Pts',(76.9272727088508,79.1823476029926,203.518749999044));
#29345=CARTESIAN_POINT('Ctrl Pts',(77.6123116091322,79.0157300353421,203.577083332377));
#29346=CARTESIAN_POINT('Ctrl Pts',(78.099126105575,79.5256823417411,203.635416665711));
#29347=CARTESIAN_POINT('Ctrl Pts',(78.5859406020177,80.0356346481401,203.693749999044));
#29348=CARTESIAN_POINT('Ctrl Pts',(78.3877161981791,80.7122045221895,203.752083332377));
#29349=CARTESIAN_POINT('Ctrl Pts',(78.1894917943405,81.388774396239,203.810416665711));
#29350=CARTESIAN_POINT('Ctrl Pts',(77.5044528940591,81.5553919638894,203.868749999044));
#29351=CARTESIAN_POINT('Origin',(77.2158628014549,80.3688697834408,198.006249999044));
#29352=CARTESIAN_POINT('',(77.5044528940591,81.5553919638894,202.468749999044));
#29353=CARTESIAN_POINT('',(77.5044528940591,81.5553919638894,202.643749999044));
#29354=CARTESIAN_POINT('',(77.504452894059,81.555391963889,198.006249999044));
#29355=CARTESIAN_POINT('Ctrl Pts',(77.5044528940591,81.5553919638894,202.643749999044));
#29356=CARTESIAN_POINT('Ctrl Pts',(76.8194139937778,81.7220095315399,202.702083332377));
#29357=CARTESIAN_POINT('Ctrl Pts',(76.332599497335,81.2120572251409,202.760416665711));
#29358=CARTESIAN_POINT('Ctrl Pts',(75.8457850008923,80.7021049187419,202.818749999044));
#29359=CARTESIAN_POINT('Ctrl Pts',(76.0440094047309,80.0255350446925,202.877083332377));
#29360=CARTESIAN_POINT('Ctrl Pts',(76.2422338085695,79.348965170643,202.935416665711));
#29361=CARTESIAN_POINT('Ctrl Pts',(76.9272727088508,79.1823476029926,202.993749999044));
#29362=CARTESIAN_POINT('Ctrl Pts',(77.6123116091322,79.0157300353421,203.052083332377));
#29363=CARTESIAN_POINT('Ctrl Pts',(78.099126105575,79.5256823417411,203.110416665711));
#29364=CARTESIAN_POINT('Ctrl Pts',(78.5859406020177,80.0356346481401,203.168749999044));
#29365=CARTESIAN_POINT('Ctrl Pts',(78.3877161981791,80.7122045221895,203.227083332377));
#29366=CARTESIAN_POINT('Ctrl Pts',(78.1894917943405,81.388774396239,203.285416665711));
#29367=CARTESIAN_POINT('Ctrl Pts',(77.5044528940591,81.5553919638894,203.343749999044));
#29368=CARTESIAN_POINT('Ctrl Pts',(77.5044528940591,81.5553919638894,202.468749999044));
#29369=CARTESIAN_POINT('Ctrl Pts',(76.8194139937778,81.7220095315399,202.527083332377));
#29370=CARTESIAN_POINT('Ctrl Pts',(76.332599497335,81.2120572251409,202.585416665711));
#29371=CARTESIAN_POINT('Ctrl Pts',(75.8457850008923,80.702104918742,202.643749999044));
#29372=CARTESIAN_POINT('Ctrl Pts',(76.0440094047309,80.0255350446925,202.702083332377));
#29373=CARTESIAN_POINT('Ctrl Pts',(76.2422338085695,79.348965170643,202.760416665711));
#29374=CARTESIAN_POINT('Ctrl Pts',(76.9272727088508,79.1823476029926,202.818749999044));
#29375=CARTESIAN_POINT('Ctrl Pts',(77.6123116091322,79.0157300353421,202.877083332377));
#29376=CARTESIAN_POINT('Ctrl Pts',(78.099126105575,79.5256823417411,202.935416665711));
#29377=CARTESIAN_POINT('Ctrl Pts',(78.5859406020177,80.0356346481401,202.993749999044));
#29378=CARTESIAN_POINT('Ctrl Pts',(78.3877161981791,80.7122045221895,203.052083332377));
#29379=CARTESIAN_POINT('Ctrl Pts',(78.1894917943405,81.388774396239,203.110416665711));
#29380=CARTESIAN_POINT('Ctrl Pts',(77.5044528940591,81.5553919638894,203.168749999044));
#29381=CARTESIAN_POINT('Origin',(77.2158628014549,80.3688697834408,198.006249999044));
#29382=CARTESIAN_POINT('',(77.5044528940591,81.5553919638894,201.768749999044));
#29383=CARTESIAN_POINT('',(77.5044528940591,81.5553919638894,201.943749999044));
#29384=CARTESIAN_POINT('',(77.504452894059,81.555391963889,198.006249999044));
#29385=CARTESIAN_POINT('Ctrl Pts',(77.5044528940591,81.5553919638894,201.943749999044));
#29386=CARTESIAN_POINT('Ctrl Pts',(76.8194139937778,81.7220095315399,202.002083332377));
#29387=CARTESIAN_POINT('Ctrl Pts',(76.332599497335,81.2120572251409,202.060416665711));
#29388=CARTESIAN_POINT('Ctrl Pts',(75.8457850008923,80.702104918742,202.118749999044));
#29389=CARTESIAN_POINT('Ctrl Pts',(76.0440094047309,80.0255350446925,202.177083332377));
#29390=CARTESIAN_POINT('Ctrl Pts',(76.2422338085695,79.348965170643,202.235416665711));
#29391=CARTESIAN_POINT('Ctrl Pts',(76.9272727088508,79.1823476029926,202.293749999044));
#29392=CARTESIAN_POINT('Ctrl Pts',(77.6123116091322,79.0157300353421,202.352083332377));
#29393=CARTESIAN_POINT('Ctrl Pts',(78.099126105575,79.5256823417411,202.410416665711));
#29394=CARTESIAN_POINT('Ctrl Pts',(78.5859406020177,80.0356346481401,202.468749999044));
#29395=CARTESIAN_POINT('Ctrl Pts',(78.3877161981791,80.7122045221895,202.527083332377));
#29396=CARTESIAN_POINT('Ctrl Pts',(78.1894917943405,81.388774396239,202.585416665711));
#29397=CARTESIAN_POINT('Ctrl Pts',(77.5044528940591,81.5553919638894,202.643749999044));
#29398=CARTESIAN_POINT('Ctrl Pts',(77.5044528940591,81.5553919638894,201.768749999044));
#29399=CARTESIAN_POINT('Ctrl Pts',(76.8194139937778,81.7220095315399,201.827083332377));
#29400=CARTESIAN_POINT('Ctrl Pts',(76.332599497335,81.2120572251409,201.885416665711));
#29401=CARTESIAN_POINT('Ctrl Pts',(75.8457850008923,80.702104918742,201.943749999044));
#29402=CARTESIAN_POINT('Ctrl Pts',(76.0440094047309,80.0255350446925,202.002083332377));
#29403=CARTESIAN_POINT('Ctrl Pts',(76.2422338085695,79.348965170643,202.060416665711));
#29404=CARTESIAN_POINT('Ctrl Pts',(76.9272727088508,79.1823476029926,202.118749999044));
#29405=CARTESIAN_POINT('Ctrl Pts',(77.6123116091322,79.0157300353421,202.177083332377));
#29406=CARTESIAN_POINT('Ctrl Pts',(78.099126105575,79.5256823417411,202.235416665711));
#29407=CARTESIAN_POINT('Ctrl Pts',(78.5859406020177,80.0356346481401,202.293749999044));
#29408=CARTESIAN_POINT('Ctrl Pts',(78.3877161981791,80.7122045221895,202.352083332377));
#29409=CARTESIAN_POINT('Ctrl Pts',(78.1894917943405,81.388774396239,202.410416665711));
#29410=CARTESIAN_POINT('Ctrl Pts',(77.5044528940591,81.5553919638894,202.468749999044));
#29411=CARTESIAN_POINT('Origin',(77.2158628014549,80.3688697834408,198.006249999044));
#29412=CARTESIAN_POINT('',(77.5044528940591,81.5553919638894,201.068749999044));
#29413=CARTESIAN_POINT('',(77.5044528940591,81.5553919638894,201.243749999044));
#29414=CARTESIAN_POINT('',(77.504452894059,81.555391963889,198.006249999044));
#29415=CARTESIAN_POINT('Ctrl Pts',(77.5044528940591,81.5553919638894,201.243749999044));
#29416=CARTESIAN_POINT('Ctrl Pts',(76.8194139937778,81.7220095315399,201.302083332377));
#29417=CARTESIAN_POINT('Ctrl Pts',(76.332599497335,81.2120572251409,201.360416665711));
#29418=CARTESIAN_POINT('Ctrl Pts',(75.8457850008923,80.702104918742,201.418749999044));
#29419=CARTESIAN_POINT('Ctrl Pts',(76.0440094047309,80.0255350446925,201.477083332377));
#29420=CARTESIAN_POINT('Ctrl Pts',(76.2422338085695,79.348965170643,201.535416665711));
#29421=CARTESIAN_POINT('Ctrl Pts',(76.9272727088508,79.1823476029926,201.593749999044));
#29422=CARTESIAN_POINT('Ctrl Pts',(77.6123116091322,79.0157300353421,201.652083332377));
#29423=CARTESIAN_POINT('Ctrl Pts',(78.099126105575,79.5256823417411,201.710416665711));
#29424=CARTESIAN_POINT('Ctrl Pts',(78.5859406020177,80.0356346481401,201.768749999044));
#29425=CARTESIAN_POINT('Ctrl Pts',(78.3877161981791,80.7122045221895,201.827083332377));
#29426=CARTESIAN_POINT('Ctrl Pts',(78.1894917943405,81.388774396239,201.885416665711));
#29427=CARTESIAN_POINT('Ctrl Pts',(77.5044528940591,81.5553919638894,201.943749999044));
#29428=CARTESIAN_POINT('Ctrl Pts',(77.5044528940591,81.5553919638894,201.068749999044));
#29429=CARTESIAN_POINT('Ctrl Pts',(76.8194139937778,81.7220095315399,201.127083332377));
#29430=CARTESIAN_POINT('Ctrl Pts',(76.332599497335,81.2120572251409,201.185416665711));
#29431=CARTESIAN_POINT('Ctrl Pts',(75.8457850008923,80.702104918742,201.243749999044));
#29432=CARTESIAN_POINT('Ctrl Pts',(76.0440094047309,80.0255350446925,201.302083332377));
#29433=CARTESIAN_POINT('Ctrl Pts',(76.2422338085695,79.348965170643,201.360416665711));
#29434=CARTESIAN_POINT('Ctrl Pts',(76.9272727088508,79.1823476029926,201.418749999044));
#29435=CARTESIAN_POINT('Ctrl Pts',(77.6123116091322,79.0157300353421,201.477083332377));
#29436=CARTESIAN_POINT('Ctrl Pts',(78.099126105575,79.5256823417411,201.535416665711));
#29437=CARTESIAN_POINT('Ctrl Pts',(78.5859406020177,80.0356346481401,201.593749999044));
#29438=CARTESIAN_POINT('Ctrl Pts',(78.3877161981791,80.7122045221895,201.652083332377));
#29439=CARTESIAN_POINT('Ctrl Pts',(78.1894917943405,81.388774396239,201.710416665711));
#29440=CARTESIAN_POINT('Ctrl Pts',(77.5044528940591,81.5553919638894,201.768749999044));
#29441=CARTESIAN_POINT('Origin',(77.2158628014549,80.3688697834408,198.006249999044));
#29442=CARTESIAN_POINT('',(77.5044528940591,81.5553919638894,200.368749999044));
#29443=CARTESIAN_POINT('',(77.5044528940591,81.5553919638894,200.543749999044));
#29444=CARTESIAN_POINT('',(77.504452894059,81.555391963889,198.006249999044));
#29445=CARTESIAN_POINT('Ctrl Pts',(77.5044528940591,81.5553919638894,200.543749999044));
#29446=CARTESIAN_POINT('Ctrl Pts',(76.8194139937778,81.7220095315399,200.602083332377));
#29447=CARTESIAN_POINT('Ctrl Pts',(76.332599497335,81.2120572251409,200.660416665711));
#29448=CARTESIAN_POINT('Ctrl Pts',(75.8457850008923,80.702104918742,200.718749999044));
#29449=CARTESIAN_POINT('Ctrl Pts',(76.0440094047309,80.0255350446925,200.777083332377));
#29450=CARTESIAN_POINT('Ctrl Pts',(76.2422338085695,79.348965170643,200.835416665711));
#29451=CARTESIAN_POINT('Ctrl Pts',(76.9272727088508,79.1823476029926,200.893749999044));
#29452=CARTESIAN_POINT('Ctrl Pts',(77.6123116091322,79.0157300353421,200.952083332377));
#29453=CARTESIAN_POINT('Ctrl Pts',(78.099126105575,79.5256823417411,201.010416665711));
#29454=CARTESIAN_POINT('Ctrl Pts',(78.5859406020177,80.0356346481401,201.068749999044));
#29455=CARTESIAN_POINT('Ctrl Pts',(78.3877161981791,80.7122045221895,201.127083332377));
#29456=CARTESIAN_POINT('Ctrl Pts',(78.1894917943405,81.388774396239,201.185416665711));
#29457=CARTESIAN_POINT('Ctrl Pts',(77.5044528940591,81.5553919638894,201.243749999044));
#29458=CARTESIAN_POINT('Ctrl Pts',(77.5044528940591,81.5553919638894,200.368749999044));
#29459=CARTESIAN_POINT('Ctrl Pts',(76.8194139937778,81.7220095315399,200.427083332377));
#29460=CARTESIAN_POINT('Ctrl Pts',(76.332599497335,81.2120572251409,200.485416665711));
#29461=CARTESIAN_POINT('Ctrl Pts',(75.8457850008923,80.702104918742,200.543749999044));
#29462=CARTESIAN_POINT('Ctrl Pts',(76.0440094047309,80.0255350446925,200.602083332377));
#29463=CARTESIAN_POINT('Ctrl Pts',(76.2422338085695,79.348965170643,200.660416665711));
#29464=CARTESIAN_POINT('Ctrl Pts',(76.9272727088508,79.1823476029926,200.718749999044));
#29465=CARTESIAN_POINT('Ctrl Pts',(77.6123116091322,79.0157300353421,200.777083332377));
#29466=CARTESIAN_POINT('Ctrl Pts',(78.099126105575,79.5256823417411,200.835416665711));
#29467=CARTESIAN_POINT('Ctrl Pts',(78.5859406020177,80.0356346481401,200.893749999044));
#29468=CARTESIAN_POINT('Ctrl Pts',(78.3877161981791,80.7122045221895,200.952083332377));
#29469=CARTESIAN_POINT('Ctrl Pts',(78.1894917943405,81.388774396239,201.010416665711));
#29470=CARTESIAN_POINT('Ctrl Pts',(77.5044528940591,81.5553919638894,201.068749999044));
#29471=CARTESIAN_POINT('Origin',(77.2158628014549,80.3688697834408,198.006249999044));
#29472=CARTESIAN_POINT('',(77.5044528940591,81.5553919638894,199.668749999044));
#29473=CARTESIAN_POINT('',(77.5044528940591,81.5553919638894,199.843749999044));
#29474=CARTESIAN_POINT('',(77.504452894059,81.555391963889,198.006249999044));
#29475=CARTESIAN_POINT('Ctrl Pts',(77.5044528940591,81.5553919638894,199.843749999044));
#29476=CARTESIAN_POINT('Ctrl Pts',(76.8194139937778,81.7220095315399,199.902083332377));
#29477=CARTESIAN_POINT('Ctrl Pts',(76.332599497335,81.2120572251409,199.960416665711));
#29478=CARTESIAN_POINT('Ctrl Pts',(75.8457850008923,80.702104918742,200.018749999044));
#29479=CARTESIAN_POINT('Ctrl Pts',(76.0440094047309,80.0255350446925,200.077083332377));
#29480=CARTESIAN_POINT('Ctrl Pts',(76.2422338085695,79.3489651706431,200.135416665711));
#29481=CARTESIAN_POINT('Ctrl Pts',(76.9272727088508,79.1823476029926,200.193749999044));
#29482=CARTESIAN_POINT('Ctrl Pts',(77.6123116091322,79.0157300353421,200.252083332377));
#29483=CARTESIAN_POINT('Ctrl Pts',(78.099126105575,79.5256823417411,200.310416665711));
#29484=CARTESIAN_POINT('Ctrl Pts',(78.5859406020177,80.0356346481401,200.368749999044));
#29485=CARTESIAN_POINT('Ctrl Pts',(78.3877161981791,80.7122045221895,200.427083332377));
#29486=CARTESIAN_POINT('Ctrl Pts',(78.1894917943405,81.388774396239,200.485416665711));
#29487=CARTESIAN_POINT('Ctrl Pts',(77.5044528940591,81.5553919638894,200.543749999044));
#29488=CARTESIAN_POINT('Ctrl Pts',(77.5044528940591,81.5553919638894,199.668749999044));
#29489=CARTESIAN_POINT('Ctrl Pts',(76.8194139937778,81.7220095315399,199.727083332377));
#29490=CARTESIAN_POINT('Ctrl Pts',(76.332599497335,81.2120572251409,199.785416665711));
#29491=CARTESIAN_POINT('Ctrl Pts',(75.8457850008923,80.702104918742,199.843749999044));
#29492=CARTESIAN_POINT('Ctrl Pts',(76.0440094047309,80.0255350446925,199.902083332377));
#29493=CARTESIAN_POINT('Ctrl Pts',(76.2422338085695,79.3489651706431,199.960416665711));
#29494=CARTESIAN_POINT('Ctrl Pts',(76.9272727088508,79.1823476029926,200.018749999044));
#29495=CARTESIAN_POINT('Ctrl Pts',(77.6123116091322,79.0157300353421,200.077083332377));
#29496=CARTESIAN_POINT('Ctrl Pts',(78.099126105575,79.5256823417411,200.135416665711));
#29497=CARTESIAN_POINT('Ctrl Pts',(78.5859406020177,80.0356346481401,200.193749999044));
#29498=CARTESIAN_POINT('Ctrl Pts',(78.3877161981791,80.7122045221895,200.252083332377));
#29499=CARTESIAN_POINT('Ctrl Pts',(78.1894917943405,81.388774396239,200.310416665711));
#29500=CARTESIAN_POINT('Ctrl Pts',(77.5044528940591,81.5553919638894,200.368749999044));
#29501=CARTESIAN_POINT('Origin',(77.2158628014549,80.3688697834408,198.006249999044));
#29502=CARTESIAN_POINT('',(77.5044528940591,81.5553919638894,198.968749999044));
#29503=CARTESIAN_POINT('',(77.5044528940591,81.5553919638894,199.143749999044));
#29504=CARTESIAN_POINT('',(77.504452894059,81.555391963889,198.006249999044));
#29505=CARTESIAN_POINT('Ctrl Pts',(77.5044528940591,81.5553919638894,199.143749999044));
#29506=CARTESIAN_POINT('Ctrl Pts',(76.8194139937778,81.7220095315399,199.202083332377));
#29507=CARTESIAN_POINT('Ctrl Pts',(76.332599497335,81.2120572251409,199.260416665711));
#29508=CARTESIAN_POINT('Ctrl Pts',(75.8457850008923,80.702104918742,199.318749999044));
#29509=CARTESIAN_POINT('Ctrl Pts',(76.0440094047309,80.0255350446925,199.377083332377));
#29510=CARTESIAN_POINT('Ctrl Pts',(76.2422338085695,79.3489651706431,199.435416665711));
#29511=CARTESIAN_POINT('Ctrl Pts',(76.9272727088509,79.1823476029926,199.493749999044));
#29512=CARTESIAN_POINT('Ctrl Pts',(77.6123116091322,79.0157300353421,199.552083332377));
#29513=CARTESIAN_POINT('Ctrl Pts',(78.099126105575,79.5256823417411,199.610416665711));
#29514=CARTESIAN_POINT('Ctrl Pts',(78.5859406020177,80.0356346481401,199.668749999044));
#29515=CARTESIAN_POINT('Ctrl Pts',(78.3877161981791,80.7122045221895,199.727083332377));
#29516=CARTESIAN_POINT('Ctrl Pts',(78.1894917943405,81.388774396239,199.785416665711));
#29517=CARTESIAN_POINT('Ctrl Pts',(77.5044528940591,81.5553919638894,199.843749999044));
#29518=CARTESIAN_POINT('Ctrl Pts',(77.5044528940591,81.5553919638894,198.968749999044));
#29519=CARTESIAN_POINT('Ctrl Pts',(76.8194139937778,81.7220095315399,199.027083332377));
#29520=CARTESIAN_POINT('Ctrl Pts',(76.332599497335,81.2120572251409,199.085416665711));
#29521=CARTESIAN_POINT('Ctrl Pts',(75.8457850008923,80.702104918742,199.143749999044));
#29522=CARTESIAN_POINT('Ctrl Pts',(76.0440094047309,80.0255350446925,199.202083332377));
#29523=CARTESIAN_POINT('Ctrl Pts',(76.2422338085695,79.3489651706431,199.260416665711));
#29524=CARTESIAN_POINT('Ctrl Pts',(76.9272727088509,79.1823476029926,199.318749999044));
#29525=CARTESIAN_POINT('Ctrl Pts',(77.6123116091322,79.0157300353421,199.377083332377));
#29526=CARTESIAN_POINT('Ctrl Pts',(78.099126105575,79.5256823417411,199.435416665711));
#29527=CARTESIAN_POINT('Ctrl Pts',(78.5859406020177,80.0356346481401,199.493749999044));
#29528=CARTESIAN_POINT('Ctrl Pts',(78.3877161981791,80.7122045221895,199.552083332377));
#29529=CARTESIAN_POINT('Ctrl Pts',(78.1894917943405,81.388774396239,199.610416665711));
#29530=CARTESIAN_POINT('Ctrl Pts',(77.5044528940591,81.5553919638894,199.668749999044));
#29531=CARTESIAN_POINT('Origin',(77.2158628014549,80.3688697834408,198.006249999044));
#29532=CARTESIAN_POINT('',(77.5044528940591,81.5553919638894,198.268749999044));
#29533=CARTESIAN_POINT('',(77.5044528940591,81.5553919638894,198.443749999044));
#29534=CARTESIAN_POINT('',(77.504452894059,81.555391963889,198.006249999044));
#29535=CARTESIAN_POINT('',(76.9272727088509,79.1823476029926,197.918749999044));
#29536=CARTESIAN_POINT('Ctrl Pts',(76.9272727088509,79.1823476029926,197.918749999044));
#29537=CARTESIAN_POINT('Ctrl Pts',(77.6123116091322,79.0157300353421,197.977083332377));
#29538=CARTESIAN_POINT('Ctrl Pts',(78.099126105575,79.5256823417411,198.035416665711));
#29539=CARTESIAN_POINT('Ctrl Pts',(78.5859406020177,80.0356346481401,198.093749999044));
#29540=CARTESIAN_POINT('Ctrl Pts',(78.3877161981791,80.7122045221895,198.152083332377));
#29541=CARTESIAN_POINT('Ctrl Pts',(78.1894917943405,81.388774396239,198.210416665711));
#29542=CARTESIAN_POINT('Ctrl Pts',(77.5044528940591,81.5553919638894,198.268749999044));
#29543=CARTESIAN_POINT('',(76.9272727088509,79.1823476029926,198.093749999044));
#29544=CARTESIAN_POINT('',(76.9272727088509,79.1823476029926,198.006249999044));
#29545=CARTESIAN_POINT('Ctrl Pts',(76.9272727088509,79.1823476029926,198.093749999044));
#29546=CARTESIAN_POINT('Ctrl Pts',(77.6123116091322,79.0157300353421,198.152083332378));
#29547=CARTESIAN_POINT('Ctrl Pts',(78.099126105575,79.5256823417411,198.210416665711));
#29548=CARTESIAN_POINT('Ctrl Pts',(78.5859406020177,80.0356346481401,198.268749999044));
#29549=CARTESIAN_POINT('Ctrl Pts',(78.3877161981791,80.7122045221895,198.327083332377));
#29550=CARTESIAN_POINT('Ctrl Pts',(78.1894917943405,81.388774396239,198.385416665711));
#29551=CARTESIAN_POINT('Ctrl Pts',(77.5044528940591,81.5553919638894,198.443749999044));
#29552=CARTESIAN_POINT('Origin',(77.215862801455,80.3688697834411,196.));
#29553=CARTESIAN_POINT('',(79.2246973681942,88.6280818332357,204.25));
#29554=CARTESIAN_POINT('',(79.2246973681943,88.6280818332357,204.062499995903));
#29555=CARTESIAN_POINT('',(79.2246973681942,88.6280818332357,196.));
#29556=CARTESIAN_POINT('',(72.3914232244021,87.3670683207337,202.950490121702));
#29557=CARTESIAN_POINT('Ctrl Pts',(72.3914232244021,87.3670683207337,202.950490121702));
#29558=CARTESIAN_POINT('Ctrl Pts',(71.8866410030934,87.0190800044125,202.967172868051));
#29559=CARTESIAN_POINT('Ctrl Pts',(71.4210052486793,86.6175094622243,202.984436404133));
#29560=CARTESIAN_POINT('Ctrl Pts',(70.5787635197524,85.715337435547,203.01975318524));
#29561=CARTESIAN_POINT('Ctrl Pts',(70.2059380614513,85.2162151353597,203.037707708689));
#29562=CARTESIAN_POINT('Ctrl Pts',(69.3281756281021,83.7251393098489,203.087330386574));
#29563=CARTESIAN_POINT('Ctrl Pts',(68.9580012473484,82.668401936068,203.116727001829));
#29564=CARTESIAN_POINT('Ctrl Pts',(68.6452620704762,80.4782567768875,203.177718055383));
#29565=CARTESIAN_POINT('Ctrl Pts',(68.7034266927971,79.3661137029368,203.209648851176));
#29566=CARTESIAN_POINT('Ctrl Pts',(69.2432554551038,77.2191089181655,203.273183071381));
#29567=CARTESIAN_POINT('Ctrl Pts',(69.7225545707681,76.205486960677,203.302726170008));
#29568=CARTESIAN_POINT('Ctrl Pts',(71.0390106890496,74.4264730124253,203.363616273261));
#29569=CARTESIAN_POINT('Ctrl Pts',(71.8610437967351,73.6762308356727,203.395503603533));
#29570=CARTESIAN_POINT('Ctrl Pts',(73.7538572107139,72.5265957263018,203.459097812285));
#29571=CARTESIAN_POINT('Ctrl Pts',(74.8084645726234,72.1414076437613,203.488789499096));
#29572=CARTESIAN_POINT('Ctrl Pts',(76.9959887135032,71.8005722002156,203.54958160803));
#29573=CARTESIAN_POINT('Ctrl Pts',(78.1073488517799,71.8442444202341,203.581425991173));
#29574=CARTESIAN_POINT('Ctrl Pts',(80.2627901024727,72.3559911613201,203.645076243339));
#29575=CARTESIAN_POINT('Ctrl Pts',(81.2851662350286,72.8236259817403,203.67491753275));
#29576=CARTESIAN_POINT('Ctrl Pts',(83.0813896544156,74.1192123802627,203.73561480348));
#29577=CARTESIAN_POINT('Ctrl Pts',(83.8408482567561,74.9308459382432,203.767416943822));
#29578=CARTESIAN_POINT('Ctrl Pts',(85.0151855726337,76.8102540662147,203.831119441553));
#29579=CARTESIAN_POINT('Ctrl Pts',(85.4142237057403,77.8628781075825,203.861110334641));
#29580=CARTESIAN_POINT('Ctrl Pts',(85.7808027993859,80.0478577829302,203.921716087211));
#29581=CARTESIAN_POINT('Ctrl Pts',(85.7503746510489,81.1583392967423,203.953476855176));
#29582=CARTESIAN_POINT('Ctrl Pts',(85.2644213488685,83.3213286029071,204.01722796243));
#29583=CARTESIAN_POINT('Ctrl Pts',(84.8075074237539,84.3517284345946,204.047367533357));
#29584=CARTESIAN_POINT('Ctrl Pts',(83.531047351044,86.1635553311158,204.107885216322));
#29585=CARTESIAN_POINT('Ctrl Pts',(82.7289789307318,86.9312925102494,204.139605627809));
#29586=CARTESIAN_POINT('Ctrl Pts',(81.0095420444879,88.0334763293615,204.198358840566));
#29587=CARTESIAN_POINT('Ctrl Pts',(80.1380923292335,88.4059227023454,204.224969648026));
#29588=CARTESIAN_POINT('Ctrl Pts',(79.2246973681942,88.6280818332357,204.25));
#29589=CARTESIAN_POINT('',(68.8559951920602,81.9059493368122,202.950490121702));
#29590=CARTESIAN_POINT('Origin',(77.215862801455,80.368869783441,202.950490121702));
#29591=CARTESIAN_POINT('Ctrl Pts',(79.2246973681943,88.6280818332357,204.062499995903));
#29592=CARTESIAN_POINT('Ctrl Pts',(79.423283621529,88.5797809871292,204.057058008559));
#29593=CARTESIAN_POINT('Ctrl Pts',(79.6203365987936,88.5242672453642,204.051529004407));
#29594=CARTESIAN_POINT('Ctrl Pts',(80.8896901414571,88.1165169205814,204.015059875846));
#29595=CARTESIAN_POINT('Ctrl Pts',(81.8845174455793,87.5609913684401,203.982464351867));
#29596=CARTESIAN_POINT('Ctrl Pts',(83.5685697934855,86.1201326713807,203.918773583326));
#29597=CARTESIAN_POINT('Ctrl Pts',(84.2518515672673,85.2605668161688,203.889436476945));
#29598=CARTESIAN_POINT('Ctrl Pts',(85.2760200246701,83.2943364473811,203.828907917564));
#29599=CARTESIAN_POINT('Ctrl Pts',(85.59287874222,82.1991688982689,203.796316107443));
#29600=CARTESIAN_POINT('Ctrl Pts',(85.7768504176493,79.9896690547137,203.732576372513));
#29601=CARTESIAN_POINT('Ctrl Pts',(85.6580421040234,78.8978746755789,203.703125859407));
#29602=CARTESIAN_POINT('Ctrl Pts',(85.002978577606,76.7790656498003,203.642686154301));
#29603=CARTESIAN_POINT('Ctrl Pts',(84.4575669291109,75.7771942401416,203.610098775639));
#29604=CARTESIAN_POINT('Ctrl Pts',(83.0334840710811,74.0768095521821,203.546313367191));
#29605=CARTESIAN_POINT('Ctrl Pts',(82.1808156244406,73.3843234751008,203.516750361292));
#29606=CARTESIAN_POINT('Ctrl Pts',(80.2239717765268,72.3390221629042,203.456395634484));
#29607=CARTESIAN_POINT('Ctrl Pts',(79.1309222146226,72.0106634510243,203.423813267573));
#29608=CARTESIAN_POINT('Ctrl Pts',(76.9217750892174,71.8044827977391,203.359985324643));
#29609=CARTESIAN_POINT('Ctrl Pts',(75.8284320666291,71.9125028996057,203.330311434025));
#29610=CARTESIAN_POINT('Ctrl Pts',(73.7018082415606,72.5471160907228,203.270037764671));
#29611=CARTESIAN_POINT('Ctrl Pts',(72.6937001635906,73.0833811311108,203.237460863907));
#29612=CARTESIAN_POINT('Ctrl Pts',(70.9787202124067,74.492326251948,203.173593367182));
#29613=CARTESIAN_POINT('Ctrl Pts',(70.2779830201882,75.3388184047491,203.143810801366));
#29614=CARTESIAN_POINT('Ctrl Pts',(69.2921616440775,77.1437362025972,203.088046020435));
#29615=CARTESIAN_POINT('Ctrl Pts',(68.9767211862975,78.0660485396747,203.060383345032));
#29616=CARTESIAN_POINT('Ctrl Pts',(68.6698040180304,79.9778001095946,203.004579469033));
#29617=CARTESIAN_POINT('Ctrl Pts',(68.680844924591,80.9533421379321,202.976845194334));
#29618=CARTESIAN_POINT('Ctrl Pts',(68.8559951920603,81.9059493368125,202.950490121702));
#29619=CARTESIAN_POINT('Origin',(77.215862801455,80.3688697834411,196.));
#29620=CARTESIAN_POINT('',(79.2246973681942,88.6280818332357,205.75));
#29621=CARTESIAN_POINT('',(79.2246973681943,88.6280818332357,205.562499995903));
#29622=CARTESIAN_POINT('',(79.2246973681942,88.6280818332357,196.));
#29623=CARTESIAN_POINT('Ctrl Pts',(79.2246973681942,88.6280818332357,204.25));
#29624=CARTESIAN_POINT('Ctrl Pts',(79.0547950240752,88.6694060781853,204.254655943656));
#29625=CARTESIAN_POINT('Ctrl Pts',(78.8834444842995,88.7055298532413,204.259376138516));
#29626=CARTESIAN_POINT('Ctrl Pts',(77.6286107155098,88.9297303181128,204.294121525883));
#29627=CARTESIAN_POINT('Ctrl Pts',(76.519059945055,88.9112969084925,204.325802721434));
#29628=CARTESIAN_POINT('Ctrl Pts',(74.3493693210737,88.448816367255,204.389640835724));
#29629=CARTESIAN_POINT('Ctrl Pts',(73.3116823951001,88.0016672512237,204.420071743722));
#29630=CARTESIAN_POINT('Ctrl Pts',(71.4858223196629,86.7425777384377,204.480423978711));
#29631=CARTESIAN_POINT('Ctrl Pts',(70.7107049238398,85.949222473407,204.512067202917));
#29632=CARTESIAN_POINT('Ctrl Pts',(69.4936797724917,84.0935283363631,204.575944076656));
#29633=CARTESIAN_POINT('Ctrl Pts',(69.0705221214295,83.0444081245762,204.606516264026));
#29634=CARTESIAN_POINT('Ctrl Pts',(68.6595137231166,80.8641421504103,204.666791215114));
#29635=CARTESIAN_POINT('Ctrl Pts',(68.6671715184264,79.755537398259,204.698397796675));
#29636=CARTESIAN_POINT('Ctrl Pts',(69.1084701239968,77.5799369350521,204.762310511639));
#29637=CARTESIAN_POINT('Ctrl Pts',(69.5467986618995,76.5356865569769,204.79302029213));
#29638=CARTESIAN_POINT('Ctrl Pts',(70.7902410520497,74.6972968893464,204.85322160152));
#29639=CARTESIAN_POINT('Ctrl Pts',(71.5757281294194,73.9156436995867,204.884792934278));
#29640=CARTESIAN_POINT('Ctrl Pts',(73.4211507565819,72.6805157070973,204.948738754213));
#29641=CARTESIAN_POINT('Ctrl Pts',(74.4687521441418,72.2470550435054,204.979581987296));
#29642=CARTESIAN_POINT('Ctrl Pts',(76.6468976599112,71.8172241620404,205.039713277092));
#29643=CARTESIAN_POINT('Ctrl Pts',(77.75457057589,71.8152712787778,205.071250802282));
#29644=CARTESIAN_POINT('Ctrl Pts',(79.935352918856,72.2375993840587,205.135227169339));
#29645=CARTESIAN_POINT('Ctrl Pts',(80.985471132995,72.6680198729736,205.166199347506));
#29646=CARTESIAN_POINT('Ctrl Pts',(82.8349758522186,73.8974710690159,205.226264197649));
#29647=CARTESIAN_POINT('Ctrl Pts',(83.6223835547801,74.6759082239084,205.257769387555));
#29648=CARTESIAN_POINT('Ctrl Pts',(84.8735979709579,76.5120935576774,205.321773917147));
#29649=CARTESIAN_POINT('Ctrl Pts',(85.3162529196888,77.5583271120912,205.352870247422));
#29650=CARTESIAN_POINT('Ctrl Pts',(85.7628018663327,79.7345273984181,205.412872176407));
#29651=CARTESIAN_POINT('Ctrl Pts',(85.7732716972006,80.841304840974,205.44434651953));
#29652=CARTESIAN_POINT('Ctrl Pts',(85.3742595987554,82.9918949455739,205.507359870613));
#29653=CARTESIAN_POINT('Ctrl Pts',(84.9707173507996,84.0160228988743,205.537859900258));
#29654=CARTESIAN_POINT('Ctrl Pts',(83.7753048448417,85.8924753032416,205.597591168971));
#29655=CARTESIAN_POINT('Ctrl Pts',(82.9805478176727,86.7174735805474,205.630115476302));
#29656=CARTESIAN_POINT('Ctrl Pts',(81.1914960263918,87.953499975151,205.692765029491));
#29657=CARTESIAN_POINT('Ctrl Pts',(80.2346455730534,88.3824386832226,205.722323737133));
#29658=CARTESIAN_POINT('Ctrl Pts',(79.2246973681942,88.6280818332357,205.75));
#29659=CARTESIAN_POINT('Ctrl Pts',(79.2246973681943,88.6280818332357,205.562499995903));
#29660=CARTESIAN_POINT('Ctrl Pts',(79.5746236203243,88.5429715410128,205.552910740839));
#29661=CARTESIAN_POINT('Ctrl Pts',(79.9194864351651,88.4355396208418,205.543059605121));
#29662=CARTESIAN_POINT('Ctrl Pts',(81.3049358839305,87.90468798277,205.501795396723));
#29663=CARTESIAN_POINT('Ctrl Pts',(82.2629315361387,87.299679234003,205.469215109508));
#29664=CARTESIAN_POINT('Ctrl Pts',(83.8639035856507,85.7760330146877,205.406049115479));
#29665=CARTESIAN_POINT('Ctrl Pts',(84.5007511559166,84.8815467321273,205.377540967558));
#29666=CARTESIAN_POINT('Ctrl Pts',(85.4170056442561,82.869327389813,205.316180072339));
#29667=CARTESIAN_POINT('Ctrl Pts',(85.6752527768043,81.7651846868092,205.283591952461));
#29668=CARTESIAN_POINT('Ctrl Pts',(85.7465099051162,79.5555383723896,205.220346699203));
#29669=CARTESIAN_POINT('Ctrl Pts',(85.5725187913987,78.4715730813878,205.191752596847));
#29670=CARTESIAN_POINT('Ctrl Pts',(84.8130090264641,76.3944131651278,205.130505297389));
#29671=CARTESIAN_POINT('Ctrl Pts',(84.221574323948,75.4259072756991,205.097911367659));
#29672=CARTESIAN_POINT('Ctrl Pts',(82.7207727390167,73.8015912345431,205.034590827215));
#29673=CARTESIAN_POINT('Ctrl Pts',(81.8360768739623,73.1517524198025,205.005903411154));
#29674=CARTESIAN_POINT('Ctrl Pts',(79.8364829948426,72.2051002983537,204.944767604828));
#29675=CARTESIAN_POINT('Ctrl Pts',(78.7345582667739,71.9303700942887,204.912169730469));
#29676=CARTESIAN_POINT('Ctrl Pts',(76.5246780325853,71.8274817001122,204.848777877421));
#29677=CARTESIAN_POINT('Ctrl Pts',(75.4385197825051,71.9859065952006,204.819990974591));
#29678=CARTESIAN_POINT('Ctrl Pts',(73.3493287236972,72.7159957160027,204.758964195714));
#29679=CARTESIAN_POINT('Ctrl Pts',(72.3711691691772,73.2945898915279,204.726364075756));
#29680=CARTESIAN_POINT('Ctrl Pts',(70.7251666730187,74.7738812984265,204.662904854891));
#29681=CARTESIAN_POINT('Ctrl Pts',(70.063223191121,75.6494689288741,204.63401347033));
#29682=CARTESIAN_POINT('Ctrl Pts',(69.0883868988755,77.6371261520451,204.573092928327));
#29683=CARTESIAN_POINT('Ctrl Pts',(68.7983523247012,78.7367775367209,204.540492090979));
#29684=CARTESIAN_POINT('Ctrl Pts',(68.6660525183857,80.9466834842794,204.476969388502));
#29685=CARTESIAN_POINT('Ctrl Pts',(68.8100623931427,82.0348832452754,204.44796967565));
#29686=CARTESIAN_POINT('Ctrl Pts',(69.5128719382302,84.1350181467491,204.387152295575));
#29687=CARTESIAN_POINT('Ctrl Pts',(70.0794714028321,85.1219503069534,204.354552097251));
#29688=CARTESIAN_POINT('Ctrl Pts',(71.5387480542039,86.7878789204938,204.290969715752));
#29689=CARTESIAN_POINT('Ctrl Pts',(72.4059527581372,87.4609796926977,204.261858928146));
#29690=CARTESIAN_POINT('Ctrl Pts',(74.3824659498379,88.4616684098053,204.201141392504));
#29691=CARTESIAN_POINT('Ctrl Pts',(75.4798478652081,88.7657554928307,204.168543020111));
#29692=CARTESIAN_POINT('Ctrl Pts',(77.4851947546304,88.9103627885004,204.110791644394));
#29693=CARTESIAN_POINT('Ctrl Pts',(78.3691374440652,88.8361741232926,204.085945457012));
#29694=CARTESIAN_POINT('Ctrl Pts',(79.2246973681943,88.6280818332357,204.062499995903));
#29695=CARTESIAN_POINT('Origin',(77.215862801455,80.3688697834411,196.));
#29696=CARTESIAN_POINT('',(79.2246973785439,88.6280818307184,207.249999999433));
#29697=CARTESIAN_POINT('',(79.2246973681942,88.6280818332357,207.062499995903));
#29698=CARTESIAN_POINT('',(79.2246973681942,88.6280818332357,196.));
#29699=CARTESIAN_POINT('Ctrl Pts',(79.2246973681942,88.6280818332357,205.75));
#29700=CARTESIAN_POINT('Ctrl Pts',(79.1755458686982,88.6400366335967,205.751346930282));
#29701=CARTESIAN_POINT('Ctrl Pts',(79.1262688644913,88.6515572453659,205.752699355763));
#29702=CARTESIAN_POINT('Ctrl Pts',(77.9698628699743,88.9110389610774,205.784485466601));
#29703=CARTESIAN_POINT('Ctrl Pts',(76.8242753044325,88.9352980517108,205.817004105249));
#29704=CARTESIAN_POINT('Ctrl Pts',(74.6339424779926,88.5404260675109,205.88113100013));
#29705=CARTESIAN_POINT('Ctrl Pts',(73.6073941539547,88.1418598722174,205.911779931708));
#29706=CARTESIAN_POINT('Ctrl Pts',(71.7242201023183,86.9551933032193,205.971422048223));
#29707=CARTESIAN_POINT('Ctrl Pts',(70.8949618400678,86.1640289638711,206.003935228454));
#29708=CARTESIAN_POINT('Ctrl Pts',(69.620934520418,84.3385238803041,206.068079312029));
#29709=CARTESIAN_POINT('Ctrl Pts',(69.1745364768424,83.3316264994655,206.098796541174));
#29710=CARTESIAN_POINT('Ctrl Pts',(68.6771272706965,81.1615714590069,206.158398447979));
#29711=CARTESIAN_POINT('Ctrl Pts',(68.6477002044747,80.0155565132701,206.190906394971));
#29712=CARTESIAN_POINT('Ctrl Pts',(69.0330778830864,77.8225891951059,206.255066316178));
#29713=CARTESIAN_POINT('Ctrl Pts',(69.427334389355,76.7939435507699,206.285847856963));
#29714=CARTESIAN_POINT('Ctrl Pts',(70.6064211219714,74.9049697459813,206.345412270952));
#29715=CARTESIAN_POINT('Ctrl Pts',(71.3944614102049,74.0720398398838,206.377915219963));
#29716=CARTESIAN_POINT('Ctrl Pts',(73.2154483653594,72.7900438620707,206.442089728917));
#29717=CARTESIAN_POINT('Ctrl Pts',(74.2208922163273,72.339435211705,206.472931710179));
#29718=CARTESIAN_POINT('Ctrl Pts',(76.3897696237588,71.8332387536346,206.532461203267));
#29719=CARTESIAN_POINT('Ctrl Pts',(77.5361354964002,71.799347654986,206.564959395507));
#29720=CARTESIAN_POINT('Ctrl Pts',(79.7313610613022,72.1765215240137,206.629147336906));
#29721=CARTESIAN_POINT('Ctrl Pts',(80.7618173201636,72.5670590561585,206.660046018682));
#29722=CARTESIAN_POINT('Ctrl Pts',(82.6557795940566,73.7396013264785,206.719543019744));
#29723=CARTESIAN_POINT('Ctrl Pts',(83.4918644198226,74.5249366555228,206.752036698882));
#29724=CARTESIAN_POINT('Ctrl Pts',(84.7807228499175,76.3420153261727,206.816237005651));
#29725=CARTESIAN_POINT('Ctrl Pts',(85.2349594869248,77.3462073878713,206.847188791585));
#29726=CARTESIAN_POINT('Ctrl Pts',(85.7487184883279,79.5140581565082,206.906655589377));
#29727=CARTESIAN_POINT('Ctrl Pts',(85.7864527063175,80.6607126246621,206.939144998628));
#29728=CARTESIAN_POINT('Ctrl Pts',(85.4163437395074,82.8578694327888,207.003356685832));
#29729=CARTESIAN_POINT('Ctrl Pts',(85.029005309143,83.8898837484398,207.034358132052));
#29730=CARTESIAN_POINT('Ctrl Pts',(83.8620951489767,85.7881249973492,207.093796878944));
#29731=CARTESIAN_POINT('Ctrl Pts',(83.0790932824303,86.6269136567377,207.12628225868));
#29732=CARTESIAN_POINT('Ctrl Pts',(81.2722283004464,87.9167784342393,207.190262047185));
#29733=CARTESIAN_POINT('Ctrl Pts',(80.2777067148035,88.3719651996675,207.221143704834));
#29734=CARTESIAN_POINT('Ctrl Pts',(79.2246973785512,88.6280818307166,207.249999999716));
#29735=CARTESIAN_POINT('Ctrl Pts',(79.2246973681942,88.6280818332357,207.062499995903));
#29736=CARTESIAN_POINT('Ctrl Pts',(79.7626736033752,88.4972333635754,207.047757485714));
#29737=CARTESIAN_POINT('Ctrl Pts',(80.2878070141477,88.3138381978238,207.032419967914));
#29738=CARTESIAN_POINT('Ctrl Pts',(81.8034440810387,87.6108494868901,206.985198722085));
#29739=CARTESIAN_POINT('Ctrl Pts',(82.7124722494979,86.9475821107349,206.952766759942));
#29740=CARTESIAN_POINT('Ctrl Pts',(84.2077811049857,85.3243310536124,206.890364902975));
#29741=CARTESIAN_POINT('Ctrl Pts',(84.7861500033284,84.3856184999572,206.862154478088));
#29742=CARTESIAN_POINT('Ctrl Pts',(85.5639568106204,82.3191697074304,206.799861643146));
#29743=CARTESIAN_POINT('Ctrl Pts',(85.7475839193358,81.2079590741808,206.767402352516));
#29744=CARTESIAN_POINT('Ctrl Pts',(85.6759637513273,79.0019994762435,206.704894189922));
#29745=CARTESIAN_POINT('Ctrl Pts',(85.4306991084728,77.9279460999686,206.67669199462));
#29746=CARTESIAN_POINT('Ctrl Pts',(84.5372763828389,75.9086662499856,206.614513511158));
#29747=CARTESIAN_POINT('Ctrl Pts',(83.8887715100878,74.9866037317871,206.58202939494));
#29748=CARTESIAN_POINT('Ctrl Pts',(82.2910355884302,73.4636121941794,206.519417470665));
#29749=CARTESIAN_POINT('Ctrl Pts',(81.3639040595534,72.8699554007518,206.49120940288));
#29750=CARTESIAN_POINT('Ctrl Pts',(79.3111974045988,72.0557329190648,206.429146835329));
#29751=CARTESIAN_POINT('Ctrl Pts',(78.2013681697702,71.8525659891692,206.396640441623));
#29752=CARTESIAN_POINT('Ctrl Pts',(75.9940307549196,71.886794457265,206.333927617057));
#29753=CARTESIAN_POINT('Ctrl Pts',(74.9173768924445,72.1132389779678,206.305699924668));
#29754=CARTESIAN_POINT('Ctrl Pts',(72.882372475416,72.9714597388853,206.243754368681));
#29755=CARTESIAN_POINT('Ctrl Pts',(71.9477061598788,73.6051938323627,206.21122825658));
#29756=CARTESIAN_POINT('Ctrl Pts',(70.3976584377957,75.177600839623,206.148417673761));
#29757=CARTESIAN_POINT('Ctrl Pts',(69.7890434344216,76.0934119573733,206.120157136224));
#29758=CARTESIAN_POINT('Ctrl Pts',(68.9393305596217,78.1323667575335,206.058329206286));
#29759=CARTESIAN_POINT('Ctrl Pts',(68.7170550880179,79.2405233244568,206.025785912758));
#29760=CARTESIAN_POINT('Ctrl Pts',(68.7147121793083,81.4489260707761,205.962880954843));
#29761=CARTESIAN_POINT('Ctrl Pts',(68.922869605621,82.5281167816675,205.93457504872));
#29762=CARTESIAN_POINT('Ctrl Pts',(69.7467658319345,84.5780988313576,205.872864873705));
#29763=CARTESIAN_POINT('Ctrl Pts',(70.3659340359109,85.5247843303221,205.840306882449));
#29764=CARTESIAN_POINT('Ctrl Pts',(71.9135396100891,87.1009227330191,205.777311132512));
#29765=CARTESIAN_POINT('Ctrl Pts',(72.8184293434143,87.723986727704,205.748948176635));
#29766=CARTESIAN_POINT('Ctrl Pts',(74.8438249563057,88.6078323869357,205.687355403308));
#29767=CARTESIAN_POINT('Ctrl Pts',(75.9500663190504,88.8485384995735,205.65478511637));
#29768=CARTESIAN_POINT('Ctrl Pts',(77.7976988006892,88.8800156615273,205.602025887436));
#29769=CARTESIAN_POINT('Ctrl Pts',(78.5213987089167,88.7991406036099,205.581772943243));
#29770=CARTESIAN_POINT('Ctrl Pts',(79.2246973681943,88.6280818332357,205.562499995903));
#29771=CARTESIAN_POINT('Origin',(77.215862801455,80.368869783441,196.656249997952));
#29772=CARTESIAN_POINT('',(79.0328184976949,87.8391824855399,207.718749997952));
#29773=CARTESIAN_POINT('',(79.0328184976949,87.8391824855399,208.093749997952));
#29774=CARTESIAN_POINT('',(79.0328184976949,87.8391824855399,196.656249997952));
#29775=CARTESIAN_POINT('',(75.3989071052151,72.8985570813421,208.468749997952));
#29776=CARTESIAN_POINT('Ctrl Pts',(79.0328184976949,87.8391824855399,207.718749997952));
#29777=CARTESIAN_POINT('Ctrl Pts',(75.9385136613175,88.5917901771535,207.812499997952));
#29778=CARTESIAN_POINT('Ctrl Pts',(73.2183357261436,86.9359602466059,207.906249997952));
#29779=CARTESIAN_POINT('Ctrl Pts',(70.4981577909697,85.2801303160583,207.999999997952));
#29780=CARTESIAN_POINT('Ctrl Pts',(69.7455500993561,82.1858254796809,208.093749997952));
#29781=CARTESIAN_POINT('Ctrl Pts',(68.9929424077425,79.0915206433035,208.187499997952));
#29782=CARTESIAN_POINT('Ctrl Pts',(70.6487723382901,76.3713427081296,208.281249997952));
#29783=CARTESIAN_POINT('Ctrl Pts',(72.3046022688377,73.6511647729557,208.374999997952));
#29784=CARTESIAN_POINT('Ctrl Pts',(75.3989071052151,72.8985570813421,208.468749997952));
#29785=CARTESIAN_POINT('',(75.3989071052151,72.8985570813421,208.843749997952));
#29786=CARTESIAN_POINT('',(75.3989071052151,72.8985570813421,208.656249997952));
#29787=CARTESIAN_POINT('Ctrl Pts',(79.0328184976949,87.8391824855399,208.093749997952));
#29788=CARTESIAN_POINT('Ctrl Pts',(75.9385136613175,88.5917901771535,208.187499997952));
#29789=CARTESIAN_POINT('Ctrl Pts',(73.2183357261436,86.9359602466059,208.281249997952));
#29790=CARTESIAN_POINT('Ctrl Pts',(70.4981577909697,85.2801303160583,208.374999997952));
#29791=CARTESIAN_POINT('Ctrl Pts',(69.7455500993561,82.1858254796809,208.468749997952));
#29792=CARTESIAN_POINT('Ctrl Pts',(68.9929424077425,79.0915206433035,208.562499997952));
#29793=CARTESIAN_POINT('Ctrl Pts',(70.6487723382901,76.3713427081296,208.656249997952));
#29794=CARTESIAN_POINT('Ctrl Pts',(72.3046022688377,73.6511647729557,208.749999997952));
#29795=CARTESIAN_POINT('Ctrl Pts',(75.3989071052151,72.8985570813421,208.843749997952));
#29796=CARTESIAN_POINT('Origin',(77.215862801455,80.368869783441,196.656249997952));
#29797=CARTESIAN_POINT('',(79.0328184976949,87.8391824855399,206.218749997952));
#29798=CARTESIAN_POINT('',(79.0328184976949,87.8391824855399,206.593749997952));
#29799=CARTESIAN_POINT('',(79.0328184976949,87.8391824855399,196.656249997952));
#29800=CARTESIAN_POINT('Ctrl Pts',(79.0328184976949,87.8391824855399,206.218749997952));
#29801=CARTESIAN_POINT('Ctrl Pts',(75.9385136613175,88.5917901771535,206.312499997952));
#29802=CARTESIAN_POINT('Ctrl Pts',(73.2183357261436,86.9359602466059,206.406249997952));
#29803=CARTESIAN_POINT('Ctrl Pts',(70.4981577909697,85.2801303160583,206.499999997952));
#29804=CARTESIAN_POINT('Ctrl Pts',(69.7455500993561,82.1858254796809,206.593749997952));
#29805=CARTESIAN_POINT('Ctrl Pts',(68.9929424077425,79.0915206433035,206.687499997952));
#29806=CARTESIAN_POINT('Ctrl Pts',(70.6487723382901,76.3713427081296,206.781249997952));
#29807=CARTESIAN_POINT('Ctrl Pts',(72.3046022688378,73.6511647729557,206.874999997952));
#29808=CARTESIAN_POINT('Ctrl Pts',(75.3989071052151,72.8985570813421,206.968749997952));
#29809=CARTESIAN_POINT('Ctrl Pts',(78.4932119415925,72.1459493897285,207.062499997952));
#29810=CARTESIAN_POINT('Ctrl Pts',(81.2133898767664,73.8017793202761,207.156249997952));
#29811=CARTESIAN_POINT('Ctrl Pts',(83.9335678119403,75.4576092508238,207.249999997952));
#29812=CARTESIAN_POINT('Ctrl Pts',(84.6861755035539,78.5519140872011,207.343749997952));
#29813=CARTESIAN_POINT('Ctrl Pts',(85.4387831951675,81.6462189235785,207.437499997952));
#29814=CARTESIAN_POINT('Ctrl Pts',(83.7829532646199,84.3663968587524,207.531249997952));
#29815=CARTESIAN_POINT('Ctrl Pts',(82.1271233340723,87.0865747939263,207.624999997952));
#29816=CARTESIAN_POINT('Ctrl Pts',(79.0328184976949,87.8391824855399,207.718749997952));
#29817=CARTESIAN_POINT('Ctrl Pts',(79.0328184976949,87.8391824855399,206.593749997952));
#29818=CARTESIAN_POINT('Ctrl Pts',(75.9385136613175,88.5917901771535,206.687499997952));
#29819=CARTESIAN_POINT('Ctrl Pts',(73.2183357261436,86.9359602466059,206.781249997952));
#29820=CARTESIAN_POINT('Ctrl Pts',(70.4981577909697,85.2801303160583,206.874999997952));
#29821=CARTESIAN_POINT('Ctrl Pts',(69.7455500993561,82.1858254796809,206.968749997952));
#29822=CARTESIAN_POINT('Ctrl Pts',(68.9929424077425,79.0915206433035,207.062499997952));
#29823=CARTESIAN_POINT('Ctrl Pts',(70.6487723382901,76.3713427081296,207.156249997952));
#29824=CARTESIAN_POINT('Ctrl Pts',(72.3046022688378,73.6511647729557,207.249999997952));
#29825=CARTESIAN_POINT('Ctrl Pts',(75.3989071052151,72.8985570813421,207.343749997952));
#29826=CARTESIAN_POINT('Ctrl Pts',(78.4932119415925,72.1459493897285,207.437499997952));
#29827=CARTESIAN_POINT('Ctrl Pts',(81.2133898767664,73.8017793202761,207.531249997952));
#29828=CARTESIAN_POINT('Ctrl Pts',(83.9335678119403,75.4576092508238,207.624999997952));
#29829=CARTESIAN_POINT('Ctrl Pts',(84.6861755035539,78.5519140872011,207.718749997952));
#29830=CARTESIAN_POINT('Ctrl Pts',(85.4387831951675,81.6462189235785,207.812499997952));
#29831=CARTESIAN_POINT('Ctrl Pts',(83.7829532646199,84.3663968587524,207.906249997952));
#29832=CARTESIAN_POINT('Ctrl Pts',(82.1271233340723,87.0865747939263,207.999999997952));
#29833=CARTESIAN_POINT('Ctrl Pts',(79.0328184976949,87.8391824855399,208.093749997952));
#29834=CARTESIAN_POINT('Origin',(77.215862801455,80.368869783441,196.656249997952));
#29835=CARTESIAN_POINT('',(79.0328184976949,87.8391824855399,204.718749997952));
#29836=CARTESIAN_POINT('',(79.0328184976949,87.8391824855399,205.093749997952));
#29837=CARTESIAN_POINT('',(79.0328184976949,87.8391824855399,196.656249997952));
#29838=CARTESIAN_POINT('Ctrl Pts',(79.0328184976949,87.8391824855399,204.718749997952));
#29839=CARTESIAN_POINT('Ctrl Pts',(75.9385136613175,88.5917901771535,204.812499997952));
#29840=CARTESIAN_POINT('Ctrl Pts',(73.2183357261436,86.9359602466059,204.906249997952));
#29841=CARTESIAN_POINT('Ctrl Pts',(70.4981577909697,85.2801303160583,204.999999997952));
#29842=CARTESIAN_POINT('Ctrl Pts',(69.7455500993561,82.1858254796809,205.093749997952));
#29843=CARTESIAN_POINT('Ctrl Pts',(68.9929424077425,79.0915206433035,205.187499997952));
#29844=CARTESIAN_POINT('Ctrl Pts',(70.6487723382901,76.3713427081296,205.281249997952));
#29845=CARTESIAN_POINT('Ctrl Pts',(72.3046022688378,73.6511647729557,205.374999997952));
#29846=CARTESIAN_POINT('Ctrl Pts',(75.3989071052151,72.8985570813421,205.468749997952));
#29847=CARTESIAN_POINT('Ctrl Pts',(78.4932119415925,72.1459493897285,205.562499997952));
#29848=CARTESIAN_POINT('Ctrl Pts',(81.2133898767664,73.8017793202761,205.656249997952));
#29849=CARTESIAN_POINT('Ctrl Pts',(83.9335678119403,75.4576092508238,205.749999997952));
#29850=CARTESIAN_POINT('Ctrl Pts',(84.6861755035539,78.5519140872011,205.843749997952));
#29851=CARTESIAN_POINT('Ctrl Pts',(85.4387831951675,81.6462189235785,205.937499997952));
#29852=CARTESIAN_POINT('Ctrl Pts',(83.7829532646199,84.3663968587524,206.031249997952));
#29853=CARTESIAN_POINT('Ctrl Pts',(82.1271233340723,87.0865747939263,206.124999997952));
#29854=CARTESIAN_POINT('Ctrl Pts',(79.0328184976949,87.8391824855399,206.218749997952));
#29855=CARTESIAN_POINT('Ctrl Pts',(79.0328184976949,87.8391824855399,205.093749997952));
#29856=CARTESIAN_POINT('Ctrl Pts',(75.9385136613175,88.5917901771535,205.187499997952));
#29857=CARTESIAN_POINT('Ctrl Pts',(73.2183357261436,86.9359602466059,205.281249997952));
#29858=CARTESIAN_POINT('Ctrl Pts',(70.4981577909697,85.2801303160583,205.374999997952));
#29859=CARTESIAN_POINT('Ctrl Pts',(69.7455500993561,82.1858254796809,205.468749997952));
#29860=CARTESIAN_POINT('Ctrl Pts',(68.9929424077425,79.0915206433035,205.562499997952));
#29861=CARTESIAN_POINT('Ctrl Pts',(70.6487723382901,76.3713427081296,205.656249997952));
#29862=CARTESIAN_POINT('Ctrl Pts',(72.3046022688378,73.6511647729557,205.749999997952));
#29863=CARTESIAN_POINT('Ctrl Pts',(75.3989071052151,72.8985570813421,205.843749997952));
#29864=CARTESIAN_POINT('Ctrl Pts',(78.4932119415925,72.1459493897285,205.937499997952));
#29865=CARTESIAN_POINT('Ctrl Pts',(81.2133898767664,73.8017793202761,206.031249997952));
#29866=CARTESIAN_POINT('Ctrl Pts',(83.9335678119403,75.4576092508238,206.124999997952));
#29867=CARTESIAN_POINT('Ctrl Pts',(84.6861755035539,78.5519140872011,206.218749997952));
#29868=CARTESIAN_POINT('Ctrl Pts',(85.4387831951675,81.6462189235785,206.312499997952));
#29869=CARTESIAN_POINT('Ctrl Pts',(83.7829532646199,84.3663968587524,206.406249997952));
#29870=CARTESIAN_POINT('Ctrl Pts',(82.1271233340723,87.0865747939263,206.499999997952));
#29871=CARTESIAN_POINT('Ctrl Pts',(79.0328184976949,87.8391824855399,206.593749997952));
#29872=CARTESIAN_POINT('Origin',(77.215862801455,80.368869783441,196.656249997952));
#29873=CARTESIAN_POINT('',(79.0328184976949,87.8391824855399,203.218749997952));
#29874=CARTESIAN_POINT('',(79.0328184976949,87.8391824855399,203.593749997952));
#29875=CARTESIAN_POINT('',(79.0328184976949,87.8391824855399,196.656249997952));
#29876=CARTESIAN_POINT('Ctrl Pts',(79.0328184976949,87.8391824855399,203.218749997952));
#29877=CARTESIAN_POINT('Ctrl Pts',(75.9385136613175,88.5917901771535,203.312499997952));
#29878=CARTESIAN_POINT('Ctrl Pts',(73.2183357261436,86.9359602466059,203.406249997952));
#29879=CARTESIAN_POINT('Ctrl Pts',(70.4981577909697,85.2801303160583,203.499999997952));
#29880=CARTESIAN_POINT('Ctrl Pts',(69.7455500993561,82.1858254796809,203.593749997952));
#29881=CARTESIAN_POINT('Ctrl Pts',(68.9929424077425,79.0915206433035,203.687499997952));
#29882=CARTESIAN_POINT('Ctrl Pts',(70.6487723382901,76.3713427081296,203.781249997952));
#29883=CARTESIAN_POINT('Ctrl Pts',(72.3046022688378,73.6511647729557,203.874999997952));
#29884=CARTESIAN_POINT('Ctrl Pts',(75.3989071052151,72.8985570813421,203.968749997952));
#29885=CARTESIAN_POINT('Ctrl Pts',(78.4932119415925,72.1459493897285,204.062499997952));
#29886=CARTESIAN_POINT('Ctrl Pts',(81.2133898767664,73.8017793202761,204.156249997952));
#29887=CARTESIAN_POINT('Ctrl Pts',(83.9335678119403,75.4576092508238,204.249999997952));
#29888=CARTESIAN_POINT('Ctrl Pts',(84.6861755035539,78.5519140872011,204.343749997952));
#29889=CARTESIAN_POINT('Ctrl Pts',(85.4387831951675,81.6462189235785,204.437499997952));
#29890=CARTESIAN_POINT('Ctrl Pts',(83.7829532646199,84.3663968587524,204.531249997952));
#29891=CARTESIAN_POINT('Ctrl Pts',(82.1271233340723,87.0865747939263,204.624999997952));
#29892=CARTESIAN_POINT('Ctrl Pts',(79.0328184976949,87.8391824855399,204.718749997952));
#29893=CARTESIAN_POINT('Ctrl Pts',(79.0328184976949,87.8391824855399,203.593749997952));
#29894=CARTESIAN_POINT('Ctrl Pts',(75.9385136613175,88.5917901771535,203.687499997952));
#29895=CARTESIAN_POINT('Ctrl Pts',(73.2183357261436,86.9359602466059,203.781249997952));
#29896=CARTESIAN_POINT('Ctrl Pts',(70.4981577909697,85.2801303160583,203.874999997952));
#29897=CARTESIAN_POINT('Ctrl Pts',(69.7455500993561,82.1858254796809,203.968749997952));
#29898=CARTESIAN_POINT('Ctrl Pts',(68.9929424077425,79.0915206433035,204.062499997952));
#29899=CARTESIAN_POINT('Ctrl Pts',(70.6487723382901,76.3713427081296,204.156249997952));
#29900=CARTESIAN_POINT('Ctrl Pts',(72.3046022688378,73.6511647729557,204.249999997952));
#29901=CARTESIAN_POINT('Ctrl Pts',(75.3989071052151,72.8985570813421,204.343749997952));
#29902=CARTESIAN_POINT('Ctrl Pts',(78.4932119415925,72.1459493897285,204.437499997952));
#29903=CARTESIAN_POINT('Ctrl Pts',(81.2133898767664,73.8017793202761,204.531249997952));
#29904=CARTESIAN_POINT('Ctrl Pts',(83.9335678119403,75.4576092508238,204.624999997952));
#29905=CARTESIAN_POINT('Ctrl Pts',(84.6861755035539,78.5519140872011,204.718749997952));
#29906=CARTESIAN_POINT('Ctrl Pts',(85.4387831951675,81.6462189235785,204.812499997952));
#29907=CARTESIAN_POINT('Ctrl Pts',(83.7829532646199,84.3663968587524,204.906249997952));
#29908=CARTESIAN_POINT('Ctrl Pts',(82.1271233340723,87.0865747939263,204.999999997952));
#29909=CARTESIAN_POINT('Ctrl Pts',(79.0328184976949,87.8391824855399,205.093749997952));
#29910=CARTESIAN_POINT('Origin',(77.215862801455,80.368869783441,196.656249997952));
#29911=CARTESIAN_POINT('',(79.0328184976949,87.8391824855399,201.718749997952));
#29912=CARTESIAN_POINT('',(79.0328184976949,87.8391824855399,202.093749997952));
#29913=CARTESIAN_POINT('',(79.0328184976949,87.8391824855399,196.656249997952));
#29914=CARTESIAN_POINT('Ctrl Pts',(79.0328184976949,87.8391824855399,201.718749997952));
#29915=CARTESIAN_POINT('Ctrl Pts',(75.9385136613175,88.5917901771536,201.812499997952));
#29916=CARTESIAN_POINT('Ctrl Pts',(73.2183357261436,86.9359602466059,201.906249997952));
#29917=CARTESIAN_POINT('Ctrl Pts',(70.4981577909697,85.2801303160583,201.999999997952));
#29918=CARTESIAN_POINT('Ctrl Pts',(69.7455500993561,82.1858254796809,202.093749997952));
#29919=CARTESIAN_POINT('Ctrl Pts',(68.9929424077425,79.0915206433035,202.187499997952));
#29920=CARTESIAN_POINT('Ctrl Pts',(70.6487723382901,76.3713427081296,202.281249997952));
#29921=CARTESIAN_POINT('Ctrl Pts',(72.3046022688378,73.6511647729557,202.374999997952));
#29922=CARTESIAN_POINT('Ctrl Pts',(75.3989071052151,72.8985570813421,202.468749997952));
#29923=CARTESIAN_POINT('Ctrl Pts',(78.4932119415925,72.1459493897285,202.562499997952));
#29924=CARTESIAN_POINT('Ctrl Pts',(81.2133898767664,73.8017793202761,202.656249997952));
#29925=CARTESIAN_POINT('Ctrl Pts',(83.9335678119403,75.4576092508238,202.749999997952));
#29926=CARTESIAN_POINT('Ctrl Pts',(84.6861755035539,78.5519140872011,202.843749997952));
#29927=CARTESIAN_POINT('Ctrl Pts',(85.4387831951675,81.6462189235785,202.937499997952));
#29928=CARTESIAN_POINT('Ctrl Pts',(83.7829532646199,84.3663968587524,203.031249997952));
#29929=CARTESIAN_POINT('Ctrl Pts',(82.1271233340723,87.0865747939263,203.124999997952));
#29930=CARTESIAN_POINT('Ctrl Pts',(79.0328184976949,87.8391824855399,203.218749997952));
#29931=CARTESIAN_POINT('Ctrl Pts',(79.0328184976949,87.8391824855399,202.093749997952));
#29932=CARTESIAN_POINT('Ctrl Pts',(75.9385136613175,88.5917901771535,202.187499997952));
#29933=CARTESIAN_POINT('Ctrl Pts',(73.2183357261436,86.9359602466059,202.281249997952));
#29934=CARTESIAN_POINT('Ctrl Pts',(70.4981577909697,85.2801303160583,202.374999997952));
#29935=CARTESIAN_POINT('Ctrl Pts',(69.7455500993561,82.1858254796809,202.468749997952));
#29936=CARTESIAN_POINT('Ctrl Pts',(68.9929424077425,79.0915206433035,202.562499997952));
#29937=CARTESIAN_POINT('Ctrl Pts',(70.6487723382901,76.3713427081296,202.656249997952));
#29938=CARTESIAN_POINT('Ctrl Pts',(72.3046022688378,73.6511647729557,202.749999997952));
#29939=CARTESIAN_POINT('Ctrl Pts',(75.3989071052151,72.8985570813421,202.843749997952));
#29940=CARTESIAN_POINT('Ctrl Pts',(78.4932119415925,72.1459493897285,202.937499997952));
#29941=CARTESIAN_POINT('Ctrl Pts',(81.2133898767664,73.8017793202761,203.031249997952));
#29942=CARTESIAN_POINT('Ctrl Pts',(83.9335678119403,75.4576092508238,203.124999997952));
#29943=CARTESIAN_POINT('Ctrl Pts',(84.6861755035539,78.5519140872011,203.218749997952));
#29944=CARTESIAN_POINT('Ctrl Pts',(85.4387831951675,81.6462189235785,203.312499997952));
#29945=CARTESIAN_POINT('Ctrl Pts',(83.7829532646199,84.3663968587524,203.406249997952));
#29946=CARTESIAN_POINT('Ctrl Pts',(82.1271233340723,87.0865747939263,203.499999997952));
#29947=CARTESIAN_POINT('Ctrl Pts',(79.0328184976949,87.8391824855399,203.593749997952));
#29948=CARTESIAN_POINT('Origin',(77.215862801455,80.368869783441,196.656249997952));
#29949=CARTESIAN_POINT('',(79.0328184976949,87.8391824855399,200.218749997952));
#29950=CARTESIAN_POINT('',(79.0328184976949,87.8391824855399,200.593749997952));
#29951=CARTESIAN_POINT('',(79.0328184976949,87.8391824855399,196.656249997952));
#29952=CARTESIAN_POINT('Ctrl Pts',(79.0328184976949,87.8391824855399,200.218749997952));
#29953=CARTESIAN_POINT('Ctrl Pts',(75.9385136613175,88.5917901771536,200.312499997952));
#29954=CARTESIAN_POINT('Ctrl Pts',(73.2183357261436,86.9359602466059,200.406249997952));
#29955=CARTESIAN_POINT('Ctrl Pts',(70.4981577909697,85.2801303160583,200.499999997952));
#29956=CARTESIAN_POINT('Ctrl Pts',(69.7455500993561,82.1858254796809,200.593749997952));
#29957=CARTESIAN_POINT('Ctrl Pts',(68.9929424077425,79.0915206433036,200.687499997952));
#29958=CARTESIAN_POINT('Ctrl Pts',(70.6487723382901,76.3713427081296,200.781249997952));
#29959=CARTESIAN_POINT('Ctrl Pts',(72.3046022688378,73.6511647729557,200.874999997952));
#29960=CARTESIAN_POINT('Ctrl Pts',(75.3989071052151,72.8985570813421,200.968749997952));
#29961=CARTESIAN_POINT('Ctrl Pts',(78.4932119415925,72.1459493897285,201.062499997952));
#29962=CARTESIAN_POINT('Ctrl Pts',(81.2133898767664,73.8017793202761,201.156249997952));
#29963=CARTESIAN_POINT('Ctrl Pts',(83.9335678119403,75.4576092508238,201.249999997952));
#29964=CARTESIAN_POINT('Ctrl Pts',(84.6861755035539,78.5519140872011,201.343749997952));
#29965=CARTESIAN_POINT('Ctrl Pts',(85.4387831951675,81.6462189235785,201.437499997952));
#29966=CARTESIAN_POINT('Ctrl Pts',(83.7829532646199,84.3663968587524,201.531249997952));
#29967=CARTESIAN_POINT('Ctrl Pts',(82.1271233340723,87.0865747939263,201.624999997952));
#29968=CARTESIAN_POINT('Ctrl Pts',(79.0328184976949,87.8391824855399,201.718749997952));
#29969=CARTESIAN_POINT('Ctrl Pts',(79.0328184976949,87.8391824855399,200.593749997952));
#29970=CARTESIAN_POINT('Ctrl Pts',(75.9385136613175,88.5917901771536,200.687499997952));
#29971=CARTESIAN_POINT('Ctrl Pts',(73.2183357261436,86.9359602466059,200.781249997952));
#29972=CARTESIAN_POINT('Ctrl Pts',(70.4981577909697,85.2801303160583,200.874999997952));
#29973=CARTESIAN_POINT('Ctrl Pts',(69.7455500993561,82.1858254796809,200.968749997952));
#29974=CARTESIAN_POINT('Ctrl Pts',(68.9929424077425,79.0915206433036,201.062499997952));
#29975=CARTESIAN_POINT('Ctrl Pts',(70.6487723382901,76.3713427081296,201.156249997952));
#29976=CARTESIAN_POINT('Ctrl Pts',(72.3046022688378,73.6511647729557,201.249999997952));
#29977=CARTESIAN_POINT('Ctrl Pts',(75.3989071052151,72.8985570813421,201.343749997952));
#29978=CARTESIAN_POINT('Ctrl Pts',(78.4932119415925,72.1459493897285,201.437499997952));
#29979=CARTESIAN_POINT('Ctrl Pts',(81.2133898767664,73.8017793202761,201.531249997952));
#29980=CARTESIAN_POINT('Ctrl Pts',(83.9335678119403,75.4576092508238,201.624999997952));
#29981=CARTESIAN_POINT('Ctrl Pts',(84.6861755035539,78.5519140872011,201.718749997952));
#29982=CARTESIAN_POINT('Ctrl Pts',(85.4387831951675,81.6462189235785,201.812499997952));
#29983=CARTESIAN_POINT('Ctrl Pts',(83.7829532646199,84.3663968587524,201.906249997952));
#29984=CARTESIAN_POINT('Ctrl Pts',(82.1271233340723,87.0865747939263,201.999999997952));
#29985=CARTESIAN_POINT('Ctrl Pts',(79.0328184976949,87.8391824855399,202.093749997952));
#29986=CARTESIAN_POINT('Origin',(77.215862801455,80.368869783441,196.656249997952));
#29987=CARTESIAN_POINT('',(79.0328184976949,87.8391824855399,198.718749997952));
#29988=CARTESIAN_POINT('',(79.0328184976949,87.8391824855399,199.093749997952));
#29989=CARTESIAN_POINT('',(79.0328184976949,87.8391824855399,196.656249997952));
#29990=CARTESIAN_POINT('Ctrl Pts',(79.0328184976949,87.8391824855399,198.718749997952));
#29991=CARTESIAN_POINT('Ctrl Pts',(75.9385136613175,88.5917901771536,198.812499997952));
#29992=CARTESIAN_POINT('Ctrl Pts',(73.2183357261436,86.9359602466059,198.906249997952));
#29993=CARTESIAN_POINT('Ctrl Pts',(70.4981577909697,85.2801303160583,198.999999997952));
#29994=CARTESIAN_POINT('Ctrl Pts',(69.7455500993561,82.1858254796809,199.093749997952));
#29995=CARTESIAN_POINT('Ctrl Pts',(68.9929424077425,79.0915206433036,199.187499997952));
#29996=CARTESIAN_POINT('Ctrl Pts',(70.6487723382901,76.3713427081296,199.281249997952));
#29997=CARTESIAN_POINT('Ctrl Pts',(72.3046022688378,73.6511647729557,199.374999997952));
#29998=CARTESIAN_POINT('Ctrl Pts',(75.3989071052151,72.8985570813421,199.468749997952));
#29999=CARTESIAN_POINT('Ctrl Pts',(78.4932119415925,72.1459493897285,199.562499997952));
#30000=CARTESIAN_POINT('Ctrl Pts',(81.2133898767664,73.8017793202761,199.656249997952));
#30001=CARTESIAN_POINT('Ctrl Pts',(83.9335678119403,75.4576092508238,199.749999997952));
#30002=CARTESIAN_POINT('Ctrl Pts',(84.6861755035539,78.5519140872012,199.843749997952));
#30003=CARTESIAN_POINT('Ctrl Pts',(85.4387831951675,81.6462189235785,199.937499997952));
#30004=CARTESIAN_POINT('Ctrl Pts',(83.7829532646199,84.3663968587524,200.031249997952));
#30005=CARTESIAN_POINT('Ctrl Pts',(82.1271233340723,87.0865747939263,200.124999997952));
#30006=CARTESIAN_POINT('Ctrl Pts',(79.0328184976949,87.8391824855399,200.218749997952));
#30007=CARTESIAN_POINT('Ctrl Pts',(79.0328184976949,87.8391824855399,199.093749997952));
#30008=CARTESIAN_POINT('Ctrl Pts',(75.9385136613175,88.5917901771536,199.187499997952));
#30009=CARTESIAN_POINT('Ctrl Pts',(73.2183357261436,86.9359602466059,199.281249997952));
#30010=CARTESIAN_POINT('Ctrl Pts',(70.4981577909697,85.2801303160583,199.374999997952));
#30011=CARTESIAN_POINT('Ctrl Pts',(69.7455500993561,82.1858254796809,199.468749997952));
#30012=CARTESIAN_POINT('Ctrl Pts',(68.9929424077425,79.0915206433036,199.562499997952));
#30013=CARTESIAN_POINT('Ctrl Pts',(70.6487723382901,76.3713427081296,199.656249997952));
#30014=CARTESIAN_POINT('Ctrl Pts',(72.3046022688378,73.6511647729557,199.749999997952));
#30015=CARTESIAN_POINT('Ctrl Pts',(75.3989071052151,72.8985570813421,199.843749997952));
#30016=CARTESIAN_POINT('Ctrl Pts',(78.4932119415925,72.1459493897285,199.937499997952));
#30017=CARTESIAN_POINT('Ctrl Pts',(81.2133898767664,73.8017793202761,200.031249997952));
#30018=CARTESIAN_POINT('Ctrl Pts',(83.9335678119403,75.4576092508238,200.124999997952));
#30019=CARTESIAN_POINT('Ctrl Pts',(84.6861755035539,78.5519140872012,200.218749997952));
#30020=CARTESIAN_POINT('Ctrl Pts',(85.4387831951675,81.6462189235785,200.312499997952));
#30021=CARTESIAN_POINT('Ctrl Pts',(83.7829532646199,84.3663968587524,200.406249997952));
#30022=CARTESIAN_POINT('Ctrl Pts',(82.1271233340723,87.0865747939263,200.499999997952));
#30023=CARTESIAN_POINT('Ctrl Pts',(79.0328184976949,87.8391824855399,200.593749997952));
#30024=CARTESIAN_POINT('Origin',(77.215862801455,80.368869783441,196.656249997952));
#30025=CARTESIAN_POINT('',(79.0328184976949,87.83918248554,197.218749997952));
#30026=CARTESIAN_POINT('',(79.0328184976949,87.83918248554,197.593749997952));
#30027=CARTESIAN_POINT('',(79.0328184976949,87.8391824855399,196.656249997952));
#30028=CARTESIAN_POINT('Ctrl Pts',(79.0328184976949,87.83918248554,197.218749997952));
#30029=CARTESIAN_POINT('Ctrl Pts',(75.9385136613175,88.5917901771536,197.312499997952));
#30030=CARTESIAN_POINT('Ctrl Pts',(73.2183357261436,86.9359602466059,197.406249997952));
#30031=CARTESIAN_POINT('Ctrl Pts',(70.4981577909697,85.2801303160583,197.499999997952));
#30032=CARTESIAN_POINT('Ctrl Pts',(69.7455500993561,82.1858254796809,197.593749997952));
#30033=CARTESIAN_POINT('Ctrl Pts',(68.9929424077425,79.0915206433036,197.687499997952));
#30034=CARTESIAN_POINT('Ctrl Pts',(70.6487723382901,76.3713427081296,197.781249997952));
#30035=CARTESIAN_POINT('Ctrl Pts',(72.3046022688378,73.6511647729557,197.874999997952));
#30036=CARTESIAN_POINT('Ctrl Pts',(75.3989071052151,72.8985570813421,197.968749997952));
#30037=CARTESIAN_POINT('Ctrl Pts',(78.4932119415925,72.1459493897285,198.062499997952));
#30038=CARTESIAN_POINT('Ctrl Pts',(81.2133898767664,73.8017793202762,198.156249997952));
#30039=CARTESIAN_POINT('Ctrl Pts',(83.9335678119403,75.4576092508238,198.249999997952));
#30040=CARTESIAN_POINT('Ctrl Pts',(84.6861755035539,78.5519140872012,198.343749997952));
#30041=CARTESIAN_POINT('Ctrl Pts',(85.4387831951675,81.6462189235785,198.437499997952));
#30042=CARTESIAN_POINT('Ctrl Pts',(83.7829532646199,84.3663968587524,198.531249997952));
#30043=CARTESIAN_POINT('Ctrl Pts',(82.1271233340723,87.0865747939263,198.624999997952));
#30044=CARTESIAN_POINT('Ctrl Pts',(79.0328184976949,87.8391824855399,198.718749997952));
#30045=CARTESIAN_POINT('Ctrl Pts',(79.0328184976949,87.83918248554,197.593749997952));
#30046=CARTESIAN_POINT('Ctrl Pts',(75.9385136613175,88.5917901771536,197.687499997952));
#30047=CARTESIAN_POINT('Ctrl Pts',(73.2183357261436,86.9359602466059,197.781249997952));
#30048=CARTESIAN_POINT('Ctrl Pts',(70.4981577909697,85.2801303160583,197.874999997952));
#30049=CARTESIAN_POINT('Ctrl Pts',(69.7455500993561,82.1858254796809,197.968749997952));
#30050=CARTESIAN_POINT('Ctrl Pts',(68.9929424077425,79.0915206433036,198.062499997952));
#30051=CARTESIAN_POINT('Ctrl Pts',(70.6487723382901,76.3713427081296,198.156249997952));
#30052=CARTESIAN_POINT('Ctrl Pts',(72.3046022688378,73.6511647729557,198.249999997952));
#30053=CARTESIAN_POINT('Ctrl Pts',(75.3989071052151,72.8985570813421,198.343749997952));
#30054=CARTESIAN_POINT('Ctrl Pts',(78.4932119415925,72.1459493897285,198.437499997952));
#30055=CARTESIAN_POINT('Ctrl Pts',(81.2133898767664,73.8017793202762,198.531249997952));
#30056=CARTESIAN_POINT('Ctrl Pts',(83.9335678119403,75.4576092508238,198.624999997952));
#30057=CARTESIAN_POINT('Ctrl Pts',(84.6861755035539,78.5519140872012,198.718749997952));
#30058=CARTESIAN_POINT('Ctrl Pts',(85.4387831951675,81.6462189235785,198.812499997952));
#30059=CARTESIAN_POINT('Ctrl Pts',(83.7829532646199,84.3663968587524,198.906249997952));
#30060=CARTESIAN_POINT('Ctrl Pts',(82.1271233340723,87.0865747939263,198.999999997952));
#30061=CARTESIAN_POINT('Ctrl Pts',(79.0328184976949,87.8391824855399,199.093749997952));
#30062=CARTESIAN_POINT('Origin',(77.215862801455,80.368869783441,202.950490121702));
#30063=CARTESIAN_POINT('',(70.3188266909529,84.6163270098801,201.781598171062));
#30064=CARTESIAN_POINT('',(70.3188266908911,84.6163270097798,202.632217951621));
#30065=CARTESIAN_POINT('',(70.3188266908911,84.6163270097798,202.950490121702));
#30066=CARTESIAN_POINT('',(71.4950332612281,74.6345773796942,202.950490121702));
#30067=CARTESIAN_POINT('Ctrl Pts',(70.3188266908911,84.6163270097798,202.632217951621));
#30068=CARTESIAN_POINT('Ctrl Pts',(69.8260630992339,83.8161757417328,202.660549743681));
#30069=CARTESIAN_POINT('Ctrl Pts',(69.4758927081056,82.9356925528463,202.687664763062));
#30070=CARTESIAN_POINT('Ctrl Pts',(69.0654723363739,80.9572904623708,202.744886064915));
#30071=CARTESIAN_POINT('Ctrl Pts',(69.0596817908794,79.8671815276535,202.777438263858));
#30072=CARTESIAN_POINT('Ctrl Pts',(69.4230173888357,78.0169388556641,202.834421549943));
#30073=CARTESIAN_POINT('Ctrl Pts',(69.6956273873066,77.2534017968305,202.858506272242));
#30074=CARTESIAN_POINT('Ctrl Pts',(70.452887584812,75.8403870443048,202.904251327559));
#30075=CARTESIAN_POINT('Ctrl Pts',(70.9308791578428,75.1974069727192,202.926669622759));
#30076=CARTESIAN_POINT('Ctrl Pts',(71.4950332612281,74.6345773796942,202.950490121702));
#30077=CARTESIAN_POINT('',(80.1444697952855,87.9209066660103,202.950490121702));
#30078=CARTESIAN_POINT('Origin',(77.215862801455,80.368869783441,202.950490121702));
#30079=CARTESIAN_POINT('Ctrl Pts',(80.1444697952855,87.9209066660103,202.950490121702));
#30080=CARTESIAN_POINT('Ctrl Pts',(80.7200382197996,87.6977067876635,202.932453294557));
#30081=CARTESIAN_POINT('Ctrl Pts',(81.2681907870714,87.4094459354855,202.913924504458));
#30082=CARTESIAN_POINT('Ctrl Pts',(82.2902634071623,86.7127185595319,202.876533681128));
#30083=CARTESIAN_POINT('Ctrl Pts',(82.7605307726769,86.3060937699065,202.857793704478));
#30084=CARTESIAN_POINT('Ctrl Pts',(83.884971986828,85.0825658474528,202.80850017344));
#30085=CARTESIAN_POINT('Ctrl Pts',(84.4354526815245,84.1863912748104,202.780263866786));
#30086=CARTESIAN_POINT('Ctrl Pts',(85.1733087176293,82.216853288982,202.717976598169));
#30087=CARTESIAN_POINT('Ctrl Pts',(85.3467097290497,81.1596354998922,202.685575488723));
#30088=CARTESIAN_POINT('Ctrl Pts',(85.2766300294487,79.0566091684042,202.623049623368));
#30089=CARTESIAN_POINT('Ctrl Pts',(85.0408547860707,78.0306016065895,202.594775699681));
#30090=CARTESIAN_POINT('Ctrl Pts',(84.1862092473497,76.1087855526369,202.532598460018));
#30091=CARTESIAN_POINT('Ctrl Pts',(83.5693696737583,75.2339905450627,202.500229467398));
#30092=CARTESIAN_POINT('Ctrl Pts',(82.0454202384975,73.782856088795,202.437597096895));
#30093=CARTESIAN_POINT('Ctrl Pts',(81.1571548977831,73.2157991039416,202.409271700632));
#30094=CARTESIAN_POINT('Ctrl Pts',(79.2002098388061,72.4445722857407,202.347205861164));
#30095=CARTESIAN_POINT('Ctrl Pts',(78.1479962948602,72.2532532406794,202.314871124405));
#30096=CARTESIAN_POINT('Ctrl Pts',(76.0437079241934,72.2862584322486,202.252135423023));
#30097=CARTESIAN_POINT('Ctrl Pts',(75.0115965537525,72.5047890330912,202.223745140531));
#30098=CARTESIAN_POINT('Ctrl Pts',(73.0753240127736,73.3271254291722,202.161791655021));
#30099=CARTESIAN_POINT('Ctrl Pts',(72.1916127489154,73.9278208919559,202.129493139258));
#30100=CARTESIAN_POINT('Ctrl Pts',(70.7136942080754,75.426517773662,202.066657580305));
#30101=CARTESIAN_POINT('Ctrl Pts',(70.1302477279942,76.3069612374748,202.038189616412));
#30102=CARTESIAN_POINT('Ctrl Pts',(69.3263609564473,78.2512964686591,201.976349011223));
#30103=CARTESIAN_POINT('Ctrl Pts',(69.1175769021875,79.2983139470911,201.944088483078));
#30104=CARTESIAN_POINT('Ctrl Pts',(69.1141855440971,81.4035063400024,201.881156792816));
#30105=CARTESIAN_POINT('Ctrl Pts',(69.3157744439333,82.4416101002022,201.852599130526));
#30106=CARTESIAN_POINT('Ctrl Pts',(69.8791381422001,83.8310072859288,201.808620460806));
#30107=CARTESIAN_POINT('Ctrl Pts',(70.0831214561213,84.2335880134999,201.795150210652));
#30108=CARTESIAN_POINT('Ctrl Pts',(70.3188266910146,84.6163270099804,201.781598171062));
#30109=CARTESIAN_POINT('Origin',(77.215862801455,80.368869783441,202.950490121702));
#30110=CARTESIAN_POINT('',(70.3188266909498,84.6163270098751,200.281598171063));
#30111=CARTESIAN_POINT('',(70.3188266908911,84.6163270097798,201.132217951621));
#30112=CARTESIAN_POINT('',(70.3188266908911,84.6163270097798,202.950490121702));
#30113=CARTESIAN_POINT('Ctrl Pts',(70.3188266908911,84.6163270097798,201.132217951621));
#30114=CARTESIAN_POINT('Ctrl Pts',(70.3172417146298,84.6137533197046,201.132309080955));
#30115=CARTESIAN_POINT('Ctrl Pts',(70.3156581350604,84.6111786711708,201.132400208759));
#30116=CARTESIAN_POINT('Ctrl Pts',(69.7713840908533,83.7251645777047,201.163747832253));
#30117=CARTESIAN_POINT('Ctrl Pts',(69.4033391753829,82.7457136988302,201.193005655864));
#30118=CARTESIAN_POINT('Ctrl Pts',(69.0500898072157,80.6632671197291,201.253601856235));
#30119=CARTESIAN_POINT('Ctrl Pts',(69.0831793119235,79.5777427661445,201.28619754089));
#30120=CARTESIAN_POINT('Ctrl Pts',(69.5626100780708,77.5205335311856,201.34990521851));
#30121=CARTESIAN_POINT('Ctrl Pts',(69.9897154545897,76.5651853971245,201.379276027556));
#30122=CARTESIAN_POINT('Ctrl Pts',(71.203353071391,74.8355585884899,201.439781139428));
#30123=CARTESIAN_POINT('Ctrl Pts',(71.9907437379569,74.086685699147,201.472372902096));
#30124=CARTESIAN_POINT('Ctrl Pts',(73.7791390912364,72.9611310339534,201.536128323692));
#30125=CARTESIAN_POINT('Ctrl Pts',(74.7548697221244,72.5824014579692,201.565611729204));
#30126=CARTESIAN_POINT('Ctrl Pts',(76.8348627554146,72.2065251754741,201.626029557126));
#30127=CARTESIAN_POINT('Ctrl Pts',(77.9218751377021,72.228201927325,201.658616729351));
#30128=CARTESIAN_POINT('Ctrl Pts',(79.9854219362805,72.6867079499083,201.72241666865));
#30129=CARTESIAN_POINT('Ctrl Pts',(80.9454462136871,73.1041483757411,201.752011531474));
#30130=CARTESIAN_POINT('Ctrl Pts',(82.688556916364,74.3009367306872,201.812345948119));
#30131=CARTESIAN_POINT('Ctrl Pts',(83.4460459700937,75.0816302105106,201.844927994003));
#30132=CARTESIAN_POINT('Ctrl Pts',(84.5898541948341,76.8602014006922,201.908769379002));
#30133=CARTESIAN_POINT('Ctrl Pts',(84.978188276254,77.8325937969514,201.938473901633));
#30134=CARTESIAN_POINT('Ctrl Pts',(85.3743549930091,79.9102875085715,201.998728813384));
#30135=CARTESIAN_POINT('Ctrl Pts',(85.3629298992261,80.9985354452161,202.0313053181));
#30136=CARTESIAN_POINT('Ctrl Pts',(84.9232223320722,83.0676784708673,202.09518523474));
#30137=CARTESIAN_POINT('Ctrl Pts',(84.5144310737503,84.0318929266988,202.124997052606));
#30138=CARTESIAN_POINT('Ctrl Pts',(83.3327545004861,85.7869845925951,202.185176368123));
#30139=CARTESIAN_POINT('Ctrl Pts',(82.5581157282637,86.5521173931964,202.21774702605));
#30140=CARTESIAN_POINT('Ctrl Pts',(80.7883960140716,87.7121957815709,202.281662719573));
#30141=CARTESIAN_POINT('Ctrl Pts',(79.8189762333589,88.1090956952885,202.311578989822));
#30142=CARTESIAN_POINT('Ctrl Pts',(77.7434069598192,88.5233170270438,202.371686591791));
#30143=CARTESIAN_POINT('Ctrl Pts',(76.6541382901548,88.5210265687059,202.404251194614));
#30144=CARTESIAN_POINT('Ctrl Pts',(74.5800853029275,88.0980732750149,202.468200068939));
#30145=CARTESIAN_POINT('Ctrl Pts',(73.6121445296276,87.6969649715002,202.498217555134));
#30146=CARTESIAN_POINT('Ctrl Pts',(71.8464791513764,86.5287362676304,202.558257275313));
#30147=CARTESIAN_POINT('Ctrl Pts',(71.0746108794289,85.7595227767601,202.590815700345));
#30148=CARTESIAN_POINT('Ctrl Pts',(70.4221941385349,84.7808451037534,202.626356078363));
#30149=CARTESIAN_POINT('Ctrl Pts',(70.3697490250245,84.6990148765756,202.629290135917));
#30150=CARTESIAN_POINT('Ctrl Pts',(70.3188266908911,84.6163270097798,202.632217951621));
#30151=CARTESIAN_POINT('Ctrl Pts',(70.3188266910146,84.6163270099805,201.781598171062));
#30152=CARTESIAN_POINT('Ctrl Pts',(70.6346499752365,85.1291619791441,201.763439687425));
#30153=CARTESIAN_POINT('Ctrl Pts',(71.0074275501507,85.6063726542895,201.745134356569));
#30154=CARTESIAN_POINT('Ctrl Pts',(72.1651851227176,86.7876714914651,201.695626618392));
#30155=CARTESIAN_POINT('Ctrl Pts',(73.0379884544506,87.3871121495928,201.666968157683));
#30156=CARTESIAN_POINT('Ctrl Pts',(74.9698735097578,88.2225480250084,201.605353172529));
#30157=CARTESIAN_POINT('Ctrl Pts',(76.0115921888612,88.4481283097861,201.573173028118));
#30158=CARTESIAN_POINT('Ctrl Pts',(78.1173401778328,88.4867821887547,201.510061026804));
#30159=CARTESIAN_POINT('Ctrl Pts',(79.1612477309362,88.3016270442561,201.481291699509));
#30160=CARTESIAN_POINT('Ctrl Pts',(81.1244989095788,87.5414248151742,201.419788608629));
#30161=CARTESIAN_POINT('Ctrl Pts',(82.0244543490064,86.9719281445366,201.387650380247));
#30162=CARTESIAN_POINT('Ctrl Pts',(83.5529616295436,85.5222393134006,201.324454466035));
#30163=CARTESIAN_POINT('Ctrl Pts',(84.1678129225914,84.6568089217546,201.29556532486));
#30164=CARTESIAN_POINT('Ctrl Pts',(85.0333440550814,82.7370483636183,201.234172975973));
#30165=CARTESIAN_POINT('Ctrl Pts',(85.2748712972383,81.7006392555677,201.202077479976));
#30166=CARTESIAN_POINT('Ctrl Pts',(85.347256719068,79.5946582363799,201.138801915413));
#30167=CARTESIAN_POINT('Ctrl Pts',(85.1778473710755,78.545202808651,201.109785196217));
#30168=CARTESIAN_POINT('Ctrl Pts',(84.4467539234772,76.5696790931711,201.048502055368));
#30169=CARTESIAN_POINT('Ctrl Pts',(83.8919287680293,75.6625209770227,201.01644985588));
#30170=CARTESIAN_POINT('Ctrl Pts',(82.4654008385435,74.1107318072355,200.953098924926));
#30171=CARTESIAN_POINT('Ctrl Pts',(81.6070029673053,73.4812132857151,200.923948082438));
#30172=CARTESIAN_POINT('Ctrl Pts',(79.698894063828,72.5873146266685,200.86277225941));
#30173=CARTESIAN_POINT('Ctrl Pts',(78.667716588934,72.330828984707,200.830763671953));
#30174=CARTESIAN_POINT('Ctrl Pts',(76.5617866497835,72.2265656625823,200.767341640629));
#30175=CARTESIAN_POINT('Ctrl Pts',(75.5070939175263,72.3810654616141,200.738051358696));
#30176=CARTESIAN_POINT('Ctrl Pts',(73.5202164800736,73.0847288407394,200.676980636246));
#30177=CARTESIAN_POINT('Ctrl Pts',(72.6065080593912,73.6257036645629,200.645015735532));
#30178=CARTESIAN_POINT('Ctrl Pts',(71.0330250648484,75.0302888775848,200.581526816573));
#30179=CARTESIAN_POINT('Ctrl Pts',(70.3897088999477,75.8820534253532,200.552092994835));
#30180=CARTESIAN_POINT('Ctrl Pts',(69.4693695179899,77.7791056656777,200.491124860899));
#30181=CARTESIAN_POINT('Ctrl Pts',(69.1990100576524,78.80520960397,200.459203492272));
#30182=CARTESIAN_POINT('Ctrl Pts',(69.0649627904852,80.9108509365622,200.395651814124));
#30183=CARTESIAN_POINT('Ctrl Pts',(69.2055019588525,81.9704299535114,200.366071533627));
#30184=CARTESIAN_POINT('Ctrl Pts',(69.7415482612329,83.5492937006154,200.317954575517));
#30185=CARTESIAN_POINT('Ctrl Pts',(70.001111301679,84.10041963382,200.299865442624));
#30186=CARTESIAN_POINT('Ctrl Pts',(70.3188266910085,84.6163270099704,200.281598171063));
#30187=CARTESIAN_POINT('Origin',(77.215862801455,80.368869783441,202.950490121702));
#30188=CARTESIAN_POINT('',(70.3188266909419,84.6163270098623,198.781598171064));
#30189=CARTESIAN_POINT('',(70.318826690899,84.6163270097926,199.63221795162));
#30190=CARTESIAN_POINT('',(70.3188266908911,84.6163270097798,202.950490121702));
#30191=CARTESIAN_POINT('Ctrl Pts',(70.3188266909068,84.6163270098053,199.63221795162));
#30192=CARTESIAN_POINT('Ctrl Pts',(70.2393441858636,84.4872630361786,199.636787854599));
#30193=CARTESIAN_POINT('Ctrl Pts',(70.1634077264338,84.3558435843596,199.641351970946));
#30194=CARTESIAN_POINT('Ctrl Pts',(69.5914552814193,83.2983166682045,199.677381204738));
#30195=CARTESIAN_POINT('Ctrl Pts',(69.2762289647801,82.2860188469412,199.706154022544));
#30196=CARTESIAN_POINT('Ctrl Pts',(69.049346466731,80.1929696435868,199.76765375273));
#30197=CARTESIAN_POINT('Ctrl Pts',(69.1416437199601,79.1319920852377,199.799790702254));
#30198=CARTESIAN_POINT('Ctrl Pts',(69.72689956906,77.1082630134724,199.862989082657));
#30199=CARTESIAN_POINT('Ctrl Pts',(70.213067098747,76.1644705992131,199.8918819662));
#30200=CARTESIAN_POINT('Ctrl Pts',(71.5204958144094,74.5136133971232,199.953270995215));
#30201=CARTESIAN_POINT('Ctrl Pts',(72.3300247830745,73.8228966637599,199.985365191647));
#30202=CARTESIAN_POINT('Ctrl Pts',(74.1529397406286,72.7989829593244,200.048149141923));
#30203=CARTESIAN_POINT('Ctrl Pts',(75.1458801342046,72.4695128292969,200.076773411079));
#30204=CARTESIAN_POINT('Ctrl Pts',(77.2362417195835,72.1983692987134,200.137987336794));
#30205=CARTESIAN_POINT('Ctrl Pts',(78.3153946330038,72.2726695921714,200.170583925419));
#30206=CARTESIAN_POINT('Ctrl Pts',(80.3487608864749,72.8276873702844,200.233929942969));
#30207=CARTESIAN_POINT('Ctrl Pts',(81.2870999465542,73.2900641784442,200.262649225009));
#30208=CARTESIAN_POINT('Ctrl Pts',(82.9666836821889,74.564801845728,200.323752854912));
#30209=CARTESIAN_POINT('Ctrl Pts',(83.6834821369912,75.3759773993898,200.35635280953));
#30210=CARTESIAN_POINT('Ctrl Pts',(84.7418259215178,77.1995991904948,200.419768590968));
#30211=CARTESIAN_POINT('Ctrl Pts',(85.0852147287464,78.1876618288599,200.448588621887));
#30212=CARTESIAN_POINT('Ctrl Pts',(85.3860521089365,80.2753408185713,200.509584521462));
#30213=CARTESIAN_POINT('Ctrl Pts',(85.3266158971152,81.3569733667024,200.542186210058));
#30214=CARTESIAN_POINT('Ctrl Pts',(84.7988723170437,83.3991143600469,200.605667849549));
#30215=CARTESIAN_POINT('Ctrl Pts',(84.349290528312,84.3436134559467,200.63459320526));
#30216=CARTESIAN_POINT('Ctrl Pts',(83.0966406729893,86.0414996244146,200.695484249101));
#30217=CARTESIAN_POINT('Ctrl Pts',(82.2939699054705,86.7700434490427,200.728086209688));
#30218=CARTESIAN_POINT('Ctrl Pts',(80.4830103856543,87.8528709165616,200.791629868083));
#30219=CARTESIAN_POINT('Ctrl Pts',(79.4994484969199,88.2091323257396,200.820664000294));
#30220=CARTESIAN_POINT('Ctrl Pts',(77.4144256644832,88.5373657539617,200.881453331427));
#30221=CARTESIAN_POINT('Ctrl Pts',(76.3306814324689,88.4916846307376,200.914054271892));
#30222=CARTESIAN_POINT('Ctrl Pts',(74.2805969035862,87.9891671339348,200.97765620027));
#30223=CARTESIAN_POINT('Ctrl Pts',(73.3304235899278,87.5513501534359,201.006801489692));
#30224=CARTESIAN_POINT('Ctrl Pts',(71.6183120197023,86.3208529792364,201.067405589061));
#30225=CARTESIAN_POINT('Ctrl Pts',(70.8807822911543,85.5288325068369,201.09990791597));
#30226=CARTESIAN_POINT('Ctrl Pts',(70.3188266908911,84.6163270097798,201.132217951621));
#30227=CARTESIAN_POINT('Ctrl Pts',(70.3188266910085,84.6163270099704,200.281598171063));
#30228=CARTESIAN_POINT('Ctrl Pts',(70.5494760509144,84.990856258714,200.26833682259));
#30229=CARTESIAN_POINT('Ctrl Pts',(70.8107716985665,85.346825340615,200.254981594731));
#30230=CARTESIAN_POINT('Ctrl Pts',(71.7956911801604,86.4807937792226,200.209714589911));
#30231=CARTESIAN_POINT('Ctrl Pts',(72.6412648242632,87.1369478572639,200.179986060603));
#30232=CARTESIAN_POINT('Ctrl Pts',(74.5279489603352,88.0816765747758,200.119214561012));
#30233=CARTESIAN_POINT('Ctrl Pts',(75.5492051502349,88.3647710802179,200.087378950053));
#30234=CARTESIAN_POINT('Ctrl Pts',(77.6543705112786,88.5263515257473,200.023713673883));
#30235=CARTESIAN_POINT('Ctrl Pts',(78.7184587991564,88.3987480480752,199.993836167195));
#30236=CARTESIAN_POINT('Ctrl Pts',(80.7251668609644,87.7442181246045,199.933158299535));
#30237=CARTESIAN_POINT('Ctrl Pts',(81.6500361236621,87.228096915081,199.901364537007));
#30238=CARTESIAN_POINT('Ctrl Pts',(83.2617789132175,85.8631001076693,199.837648139127));
#30239=CARTESIAN_POINT('Ctrl Pts',(83.9297566222614,85.0232472997634,199.807621908919));
#30240=CARTESIAN_POINT('Ctrl Pts',(84.8967679163405,83.1461787161077,199.747034333491));
#30241=CARTESIAN_POINT('Ctrl Pts',(85.1914422263021,82.1294915496872,199.715281513417));
#30242=CARTESIAN_POINT('Ctrl Pts',(85.3782270383223,80.0249398293957,199.65151756514));
#30243=CARTESIAN_POINT('Ctrl Pts',(85.2624934312454,78.9567316649269,199.621343760249));
#30244=CARTESIAN_POINT('Ctrl Pts',(84.6211639777199,76.9150092839013,199.560046631192));
#30245=CARTESIAN_POINT('Ctrl Pts',(84.0974234210483,75.963003022243,199.527454303479));
#30246=CARTESIAN_POINT('Ctrl Pts',(82.7337030830622,74.3489818669681,199.46370506325));
#30247=CARTESIAN_POINT('Ctrl Pts',(81.9184130962896,73.6926772458593,199.43423663281));
#30248=CARTESIAN_POINT('Ctrl Pts',(80.0498760145395,72.7048473490567,199.373807380033));
#30249=CARTESIAN_POINT('Ctrl Pts',(79.0073788716093,72.3964650338568,199.341219561468));
#30250=CARTESIAN_POINT('Ctrl Pts',(76.9019593562372,72.2087547767503,199.277425381815));
#30251=CARTESIAN_POINT('Ctrl Pts',(75.8606373243966,72.3159647763489,199.247845301973));
#30252=CARTESIAN_POINT('Ctrl Pts',(73.8370986097,72.9288433392431,199.187499979936));
#30253=CARTESIAN_POINT('Ctrl Pts',(72.8788631864418,73.443527337106,199.154917223455));
#30254=CARTESIAN_POINT('Ctrl Pts',(71.2503195670516,74.7922455908759,199.091081197233));
#30255=CARTESIAN_POINT('Ctrl Pts',(70.5858156746814,75.6013956219914,199.061391182953));
#30256=CARTESIAN_POINT('Ctrl Pts',(69.5792063812086,77.461529421012,199.001125887885));
#30257=CARTESIAN_POINT('Ctrl Pts',(69.2606031890589,78.5020856953131,198.968548623791));
#30258=CARTESIAN_POINT('Ctrl Pts',(69.0531349771153,80.6071381987141,198.904673686263));
#30259=CARTESIAN_POINT('Ctrl Pts',(69.1507593252483,81.6498393210891,198.874876031648));
#30260=CARTESIAN_POINT('Ctrl Pts',(69.6458614565071,83.3402031113327,198.824767605201));
#30261=CARTESIAN_POINT('Ctrl Pts',(69.9409909796789,84.0027960417003,198.803322103162));
#30262=CARTESIAN_POINT('Ctrl Pts',(70.3188266909927,84.6163270099447,198.781598171064));
#30263=CARTESIAN_POINT('Origin',(77.215862801455,80.368869783441,202.950490121702));
#30264=CARTESIAN_POINT('',(70.318826690926,84.6163270098365,197.281598171066));
#30265=CARTESIAN_POINT('',(70.3188266909362,84.6163270098531,198.132217951616));
#30266=CARTESIAN_POINT('',(70.3188266908911,84.6163270097798,202.950490121702));
#30267=CARTESIAN_POINT('',(75.3015616260917,72.4983265359896,196.230940107676));
#30268=CARTESIAN_POINT('Ctrl Pts',(70.3188266909609,84.6163270098932,197.281598171066));
#30269=CARTESIAN_POINT('Ctrl Pts',(70.4672117059276,84.8572751235334,197.273066669429));
#30270=CARTESIAN_POINT('Ctrl Pts',(70.6284024015044,85.0907395806919,197.264489304094));
#30271=CARTESIAN_POINT('Ctrl Pts',(71.4368717282468,86.1389942955801,197.224464651716));
#30272=CARTESIAN_POINT('Ctrl Pts',(72.2244576005149,86.8323619240314,197.193856836177));
#30273=CARTESIAN_POINT('Ctrl Pts',(74.0544848742302,87.9044441075959,197.134187348814));
#30274=CARTESIAN_POINT('Ctrl Pts',(75.0875048590491,88.2586825940275,197.101669877795));
#30275=CARTESIAN_POINT('Ctrl Pts',(77.1905611236561,88.5353160193394,197.037533500101));
#30276=CARTESIAN_POINT('Ctrl Pts',(78.2381050913792,88.4711088330216,197.006855826311));
#30277=CARTESIAN_POINT('Ctrl Pts',(80.2918553536182,87.9397354292445,196.947227736429));
#30278=CARTESIAN_POINT('Ctrl Pts',(81.2740996783364,87.4618459870212,196.914715572296));
#30279=CARTESIAN_POINT('Ctrl Pts',(82.959969005163,86.1737918459698,196.850562764639));
#30280=CARTESIAN_POINT('Ctrl Pts',(83.6571133639445,85.3890222970249,196.819819237289));
#30281=CARTESIAN_POINT('Ctrl Pts',(84.7376864138108,83.562991640004,196.76022977423));
#30282=CARTESIAN_POINT('Ctrl Pts',(85.0965441593794,82.5310366958102,196.727722688161));
#30283=CARTESIAN_POINT('Ctrl Pts',(85.3821786975059,80.4283223688934,196.663554741923));
#30284=CARTESIAN_POINT('Ctrl Pts',(85.3223066388472,79.3801465048748,196.632749261312));
#30285=CARTESIAN_POINT('Ctrl Pts',(84.7991430709567,77.3234506679724,196.573195798819));
#30286=CARTESIAN_POINT('Ctrl Pts',(84.3249937825088,76.3388782270904,196.540693554184));
#30287=CARTESIAN_POINT('Ctrl Pts',(83.0430855394691,74.6473245170452,196.476511663731));
#30288=CARTESIAN_POINT('Ctrl Pts',(82.2607486008549,73.9469168163812,196.445648007422));
#30289=CARTESIAN_POINT('Ctrl Pts',(80.4381814533099,72.8590216837296,196.386128062267));
#30290=CARTESIAN_POINT('Ctrl Pts',(79.4071611147434,72.4961812791765,196.353630418377));
#30291=CARTESIAN_POINT('Ctrl Pts',(77.3236635410519,72.205417441165,196.290012972736));
#30292=CARTESIAN_POINT('Ctrl Pts',(76.2942419888476,72.2568833311894,196.259486529753));
#30293=CARTESIAN_POINT('Ctrl Pts',(75.3015616260917,72.4983265359896,196.230940107676));
#30294=CARTESIAN_POINT('',(75.3015616260917,72.4983265359896,197.081559888227));
#30295=CARTESIAN_POINT('',(75.3015616260917,72.4983265359896,202.950490121702));
#30296=CARTESIAN_POINT('Ctrl Pts',(75.3015616260917,72.4983265359896,197.081559888227));
#30297=CARTESIAN_POINT('Ctrl Pts',(76.1388972823187,72.2946668163879,197.105639076212));
#30298=CARTESIAN_POINT('Ctrl Pts',(77.0033661482917,72.2259366208603,197.131155580565));
#30299=CARTESIAN_POINT('Ctrl Pts',(78.7315041943876,72.364297891176,197.18344519351));
#30300=CARTESIAN_POINT('Ctrl Pts',(79.5837955806926,72.5737898395195,197.209889408713));
#30301=CARTESIAN_POINT('Ctrl Pts',(81.3413422722311,73.321337767,197.265886083455));
#30302=CARTESIAN_POINT('Ctrl Pts',(82.2095133426904,73.9073883603634,197.294186427988));
#30303=CARTESIAN_POINT('Ctrl Pts',(83.6976207414577,75.3955000355644,197.35708183513));
#30304=CARTESIAN_POINT('Ctrl Pts',(84.2954742747404,76.2912814451157,197.389624320124));
#30305=CARTESIAN_POINT('Ctrl Pts',(85.0989511242683,78.2369163591494,197.451469750634));
#30306=CARTESIAN_POINT('Ctrl Pts',(85.3070670685511,79.2640083597879,197.479726448372));
#30307=CARTESIAN_POINT('Ctrl Pts',(85.3243366751421,81.3680350452673,197.542527381558));
#30308=CARTESIAN_POINT('Ctrl Pts',(85.1226940733133,82.4250130682218,197.575052437086));
#30309=CARTESIAN_POINT('Ctrl Pts',(84.3318171518148,84.3754507528462,197.637015022373));
#30310=CARTESIAN_POINT('Ctrl Pts',(83.7597793243371,85.2542205198593,197.665240601487));
#30311=CARTESIAN_POINT('Ctrl Pts',(82.2969958342311,86.7661999260792,197.727943723931));
#30312=CARTESIAN_POINT('Ctrl Pts',(81.4129558227272,87.37801921126,197.760448825333));
#30313=CARTESIAN_POINT('Ctrl Pts',(79.4819616351216,88.2146112337875,197.822527899281));
#30314=CARTESIAN_POINT('Ctrl Pts',(78.4573165640372,88.4404033069567,197.850735560505));
#30315=CARTESIAN_POINT('Ctrl Pts',(76.3544674416585,88.4928955888731,197.913337779465));
#30316=CARTESIAN_POINT('Ctrl Pts',(75.2960506701693,88.3096588978678,197.945820383995));
#30317=CARTESIAN_POINT('Ctrl Pts',(73.3325354514835,87.5530310304496,198.008014804058));
#30318=CARTESIAN_POINT('Ctrl Pts',(72.4428601018535,86.9953958706751,198.036218254823));
#30319=CARTESIAN_POINT('Ctrl Pts',(71.1549043755846,85.7908277885468,198.088618145068));
#30320=CARTESIAN_POINT('Ctrl Pts',(70.696419591884,85.2294637017675,198.110507980075));
#30321=CARTESIAN_POINT('Ctrl Pts',(70.3188266909814,84.6163270099265,198.132217951616));
#30322=CARTESIAN_POINT('Origin',(77.215862801455,80.368869783441,202.950490121702));
#30323=CARTESIAN_POINT('Ctrl Pts',(70.3188266909814,84.6163270099264,198.132217951616));
#30324=CARTESIAN_POINT('Ctrl Pts',(70.1413522775646,84.3281434279028,198.14242196884));
#30325=CARTESIAN_POINT('Ctrl Pts',(69.9817464533539,84.0285235129716,198.152586256108));
#30326=CARTESIAN_POINT('Ctrl Pts',(69.4105242617287,82.7711208473259,198.19348250062));
#30327=CARTESIAN_POINT('Ctrl Pts',(69.166673393273,81.74896734013,198.22169577383));
#30328=CARTESIAN_POINT('Ctrl Pts',(69.0784407110988,79.6475902217734,198.284088075341));
#30329=CARTESIAN_POINT('Ctrl Pts',(69.2430030358506,78.5880302005555,198.316518151265));
#30330=CARTESIAN_POINT('Ctrl Pts',(69.9647537190728,76.6115536643663,198.378938016748));
#30331=CARTESIAN_POINT('Ctrl Pts',(70.5077748665416,75.7108053684881,198.407175252907));
#30332=CARTESIAN_POINT('Ctrl Pts',(71.9180205367237,74.1504457791517,198.469459225153));
#30333=CARTESIAN_POINT('Ctrl Pts',(72.777309908536,73.5106505239144,198.501859398185));
#30334=CARTESIAN_POINT('Ctrl Pts',(74.6773605643387,72.6065204667344,198.564388520805));
#30335=CARTESIAN_POINT('Ctrl Pts',(75.69700422083,72.3444613591024,198.592663796792));
#30336=CARTESIAN_POINT('Ctrl Pts',(77.7966308120636,72.2204529179664,198.654837692736));
#30337=CARTESIAN_POINT('Ctrl Pts',(78.8570154818378,72.3663330781034,198.687205682111));
#30338=CARTESIAN_POINT('Ctrl Pts',(80.8461512194974,73.0530460903665,198.749841218891));
#30339=CARTESIAN_POINT('Ctrl Pts',(81.7579907861586,73.581429485084,198.778168379625));
#30340=CARTESIAN_POINT('Ctrl Pts',(83.3422023416221,74.9651645597405,198.840230840417));
#30341=CARTESIAN_POINT('Ctrl Pts',(83.9956095848265,75.8117785632511,198.872564511952));
#30342=CARTESIAN_POINT('Ctrl Pts',(84.9332439357261,77.6959210616337,198.935303278946));
#30343=CARTESIAN_POINT('Ctrl Pts',(85.2134215592527,78.713067021492,198.963695721928));
#30344=CARTESIAN_POINT('Ctrl Pts',(85.3727593018409,80.8106928555144,199.025645806591));
#30345=CARTESIAN_POINT('Ctrl Pts',(85.2453091984721,81.8715783097193,199.0579432008));
#30346=CARTESIAN_POINT('Ctrl Pts',(84.5933209928205,83.8728999526277,199.120781716382));
#30347=CARTESIAN_POINT('Ctrl Pts',(84.0794091641949,84.7957027711809,199.149252215542));
#30348=CARTESIAN_POINT('Ctrl Pts',(82.7218679072689,86.4031226790794,199.211089410695));
#30349=CARTESIAN_POINT('Ctrl Pts',(81.8878888578483,87.0696489005427,199.243348767287));
#30350=CARTESIAN_POINT('Ctrl Pts',(80.0196578434461,88.0400144799904,199.306283298298));
#30351=CARTESIAN_POINT('Ctrl Pts',(79.0049690157344,88.3379869113588,199.334843844877));
#30352=CARTESIAN_POINT('Ctrl Pts',(76.9095526933233,88.5317517568567,199.39656806787));
#30353=CARTESIAN_POINT('Ctrl Pts',(75.8484785462801,88.4222349338808,199.428787846007));
#30354=CARTESIAN_POINT('Ctrl Pts',(73.8355883492947,87.804203559603,199.491814455515));
#30355=CARTESIAN_POINT('Ctrl Pts',(72.9020920155522,87.3044176972546,199.520476119952));
#30356=CARTESIAN_POINT('Ctrl Pts',(71.3900198791337,86.0685626015633,199.577640350897));
#30357=CARTESIAN_POINT('Ctrl Pts',(70.7916687049813,85.3841295495084,199.605031564789));
#30358=CARTESIAN_POINT('Ctrl Pts',(70.3188266909068,84.6163270098053,199.63221795162));
#30359=CARTESIAN_POINT('Ctrl Pts',(70.3188266909927,84.6163270099447,198.781598171064));
#30360=CARTESIAN_POINT('Ctrl Pts',(70.5038298807908,84.9167358457598,198.770961281504));
#30361=CARTESIAN_POINT('Ctrl Pts',(70.7086598717006,85.205383306225,198.760257644138));
#30362=CARTESIAN_POINT('Ctrl Pts',(71.587249389392,86.2854632173503,198.71820432847));
#30363=CARTESIAN_POINT('Ctrl Pts',(72.390925193891,86.9572847581389,198.68830181755));
#30364=CARTESIAN_POINT('Ctrl Pts',(74.2435020092774,87.9805881515105,198.628184868632));
#30365=CARTESIAN_POINT('Ctrl Pts',(75.2822503678208,88.308278486667,198.595619448935));
#30366=CARTESIAN_POINT('Ctrl Pts',(77.3869003895154,88.533341078713,198.531674857992));
#30367=CARTESIAN_POINT('Ctrl Pts',(78.4308312232629,88.4442368646137,198.501670679398));
#30368=CARTESIAN_POINT('Ctrl Pts',(80.4673097402838,87.8656830225203,198.441622119844));
#30369=CARTESIAN_POINT('Ctrl Pts',(81.43585444097,87.366416915855,198.409062866107));
#30370=CARTESIAN_POINT('Ctrl Pts',(83.0887376501164,86.0431687325628,198.345087217402));
#30371=CARTESIAN_POINT('Ctrl Pts',(83.7670434343762,85.244339479377,198.314984884182));
#30372=CARTESIAN_POINT('Ctrl Pts',(84.8050863821067,83.3985028320405,198.255000943989));
#30373=CARTESIAN_POINT('Ctrl Pts',(85.1407999985339,82.361415368789,198.222447913808));
#30374=CARTESIAN_POINT('Ctrl Pts',(85.381420595943,80.2571809134547,198.158443514381));
#30375=CARTESIAN_POINT('Ctrl Pts',(85.2998387937799,79.212161411866,198.12824678984));
#30376=CARTESIAN_POINT('Ctrl Pts',(84.7355441492512,77.1704006602766,198.068323787707));
#30377=CARTESIAN_POINT('Ctrl Pts',(84.2427169191899,76.1976580453656,198.035776973544));
#30378=CARTESIAN_POINT('Ctrl Pts',(82.930082792761,74.5347482518195,197.971745981676));
#30379=CARTESIAN_POINT('Ctrl Pts',(82.1355176169891,73.8507332996321,197.941458811811));
#30380=CARTESIAN_POINT('Ctrl Pts',(80.2956487101043,72.7997548517861,197.881593170842));
#30381=CARTESIAN_POINT('Ctrl Pts',(79.2600688353045,72.4570005266266,197.849052510037));
#30382=CARTESIAN_POINT('Ctrl Pts',(77.1562459994661,72.2027080806856,197.784996940664));
#30383=CARTESIAN_POINT('Ctrl Pts',(76.1102688351415,72.2776878585382,197.754623393498));
#30384=CARTESIAN_POINT('Ctrl Pts',(74.0639176042385,72.829470336233,197.694811653939));
#30385=CARTESIAN_POINT('Ctrl Pts',(73.0875324344894,73.3166318441385,197.662277037938));
#30386=CARTESIAN_POINT('Ctrl Pts',(71.4158653900587,74.6199362622047,197.598198768693));
#30387=CARTESIAN_POINT('Ctrl Pts',(70.726852071004,75.4107705712388,197.567742980565));
#30388=CARTESIAN_POINT('Ctrl Pts',(69.6645815554747,77.2453897532126,197.507981809798));
#30389=CARTESIAN_POINT('Ctrl Pts',(69.3156818670123,78.279615370696,197.475453092547));
#30390=CARTESIAN_POINT('Ctrl Pts',(69.049440848975,80.3830427593049,197.411353870224));
#30391=CARTESIAN_POINT('Ctrl Pts',(69.1186568230227,81.4298576069505,197.380819998922));
#30392=CARTESIAN_POINT('Ctrl Pts',(69.5870600798276,83.2055036450499,197.329105944861));
#30393=CARTESIAN_POINT('Ctrl Pts',(69.9025454780671,83.9403680998025,197.305532554534));
#30394=CARTESIAN_POINT('Ctrl Pts',(70.3188266909609,84.6163270098932,197.281598171066));
#30395=CARTESIAN_POINT('Origin',(77.215862801455,80.368869783441,202.750490121702));
#30396=CARTESIAN_POINT('',(81.6703452938459,91.5114720703838,202.750490121702));
#30397=CARTESIAN_POINT('',(85.1614376461066,89.3615245854469,202.750490121702));
#30398=CARTESIAN_POINT('Origin',(77.215862801455,80.368869783441,202.750490121702));
#30399=CARTESIAN_POINT('',(85.1490627147209,89.3414301279668,202.750490121702));
#30400=CARTESIAN_POINT('',(85.1490627147209,89.3414301279668,202.750490121702));
#30401=CARTESIAN_POINT('',(81.6579703624602,91.4913776129038,202.750490121702));
#30402=CARTESIAN_POINT('',(85.1490627147209,89.3414301279668,202.750490121702));
#30403=CARTESIAN_POINT('',(81.6579703624602,91.4913776129038,202.750490121702));
#30404=CARTESIAN_POINT('Origin',(85.1490627147209,89.3414301279668,192.750490121702));
#30405=CARTESIAN_POINT('',(85.1490627147209,89.3414301279668,196.17168857984));
#30406=CARTESIAN_POINT('',(81.6579703624602,91.4913776129038,196.17168857984));
#30407=CARTESIAN_POINT('Ctrl Pts',(85.1490627147208,89.3414301279668,196.17168857984));
#30408=CARTESIAN_POINT('Ctrl Pts',(83.4035165385905,90.4164038704353,195.897880393518));
#30409=CARTESIAN_POINT('Ctrl Pts',(81.6579703624602,91.4913776129037,196.17168857984));
#30410=CARTESIAN_POINT('',(81.6579703624602,91.4913776129038,192.750490121702));
#30411=CARTESIAN_POINT('',(85.1490627147209,89.3414301279668,192.750490121702));
#30412=CARTESIAN_POINT('Origin',(85.1490627147209,89.3414301279668,192.750490121702));
#30413=CARTESIAN_POINT('',(86.223563176935,91.0862077899414,197.750490121702));
#30414=CARTESIAN_POINT('Ctrl Pts',(86.223563176935,91.0862077899414,197.750490121702));
#30415=CARTESIAN_POINT('Ctrl Pts',(85.6444681226414,90.1458711866332,196.898024398674));
#30416=CARTESIAN_POINT('Ctrl Pts',(85.1490627147209,89.3414301279668,196.17168857984));
#30417=CARTESIAN_POINT('',(86.223563176935,91.0862077899414,202.750490121702));
#30418=CARTESIAN_POINT('',(85.1490627147209,89.3414301279668,202.750490121702));
#30419=CARTESIAN_POINT('',(86.223563176935,91.0862077899414,202.950490121702));
#30420=CARTESIAN_POINT('Origin',(81.6579703624602,91.4913776129038,192.750490121702));
#30421=CARTESIAN_POINT('',(82.7324708246743,93.2361552748783,197.750490121702));
#30422=CARTESIAN_POINT('Ctrl Pts',(81.6579703624601,91.4913776129037,196.17168857984));
#30423=CARTESIAN_POINT('Ctrl Pts',(82.1533757703807,92.2958186715703,196.898024398674));
#30424=CARTESIAN_POINT('Ctrl Pts',(82.7324708246743,93.2361552748783,197.750490121702));
#30425=CARTESIAN_POINT('',(82.7324708246743,93.2361552748783,202.750490121702));
#30426=CARTESIAN_POINT('',(82.7324708246743,93.2361552748783,202.950490121702));
#30427=CARTESIAN_POINT('',(81.6579703624602,91.4913776129038,202.750490121702));
#30428=CARTESIAN_POINT('Origin',(77.215862801455,80.368869783441,202.750490121702));
#30429=CARTESIAN_POINT('',(86.1884231459808,72.435669870175,202.750490121702));
#30430=CARTESIAN_POINT('',(86.2085176034608,72.4232949387893,202.750490121702));
#30431=CARTESIAN_POINT('',(86.1884231459808,72.435669870175,202.750490121702));
#30432=CARTESIAN_POINT('',(88.3383706309178,75.9267622224358,202.750490121702));
#30433=CARTESIAN_POINT('',(86.1884231459808,72.435669870175,202.750490121702));
#30434=CARTESIAN_POINT('',(88.3584650883978,75.9143872910501,202.750490121702));
#30435=CARTESIAN_POINT('',(88.3383706309178,75.9267622224358,202.750490121702));
#30436=CARTESIAN_POINT('Origin',(77.215862801455,80.368869783441,202.750490121702));
#30437=CARTESIAN_POINT('Origin',(88.3383706309178,75.9267622224358,192.750490121702));
#30438=CARTESIAN_POINT('',(88.3383706309178,75.9267622224358,196.17168857984));
#30439=CARTESIAN_POINT('',(90.0831482928923,74.8522617602217,197.750490121702));
#30440=CARTESIAN_POINT('Ctrl Pts',(88.3383706309177,75.9267622224358,196.17168857984));
#30441=CARTESIAN_POINT('Ctrl Pts',(89.1428116895835,75.4313568145157,196.898024398673));
#30442=CARTESIAN_POINT('Ctrl Pts',(90.0831482928923,74.8522617602217,197.750490121702));
#30443=CARTESIAN_POINT('',(90.0831482928923,74.8522617602217,202.750490121702));
#30444=CARTESIAN_POINT('',(90.0831482928923,74.8522617602217,202.950490121702));
#30445=CARTESIAN_POINT('',(88.3383706309178,75.9267622224358,202.750490121702));
#30446=CARTESIAN_POINT('',(88.3383706309178,75.9267622224358,192.750490121702));
#30447=CARTESIAN_POINT('Origin',(86.1884231459808,72.435669870175,192.750490121702));
#30448=CARTESIAN_POINT('',(86.1884231459808,72.435669870175,196.17168857984));
#30449=CARTESIAN_POINT('Ctrl Pts',(86.1884231459808,72.435669870175,196.17168857984));
#30450=CARTESIAN_POINT('Ctrl Pts',(87.2633968884493,74.1812160463054,195.897880393518));
#30451=CARTESIAN_POINT('Ctrl Pts',(88.3383706309177,75.9267622224357,196.17168857984));
#30452=CARTESIAN_POINT('',(86.1884231459808,72.435669870175,192.750490121702));
#30453=CARTESIAN_POINT('Origin',(86.1884231459808,72.435669870175,192.750490121702));
#30454=CARTESIAN_POINT('',(87.9332008079553,71.3611694079609,197.750490121702));
#30455=CARTESIAN_POINT('Ctrl Pts',(87.9332008079553,71.3611694079609,197.750490121702));
#30456=CARTESIAN_POINT('Ctrl Pts',(86.9928642046467,71.9402644622549,196.898024398673));
#30457=CARTESIAN_POINT('Ctrl Pts',(86.1884231459808,72.435669870175,196.17168857984));
#30458=CARTESIAN_POINT('',(87.9332008079553,71.3611694079609,202.750490121702));
#30459=CARTESIAN_POINT('',(86.1884231459808,72.435669870175,202.750490121702));
#30460=CARTESIAN_POINT('',(87.9332008079553,71.3611694079609,202.950490121702));
#30461=CARTESIAN_POINT('Origin',(77.215862801455,80.368869783441,202.750490121702));
#30462=CARTESIAN_POINT('',(69.2826628881893,71.396309438915,202.750490121702));
#30463=CARTESIAN_POINT('',(69.2702879568036,71.3762149814349,202.750490121702));
#30464=CARTESIAN_POINT('',(69.2826628881893,71.396309438915,202.750490121702));
#30465=CARTESIAN_POINT('',(72.7737552404501,69.2463619539781,202.750490121702));
#30466=CARTESIAN_POINT('',(69.2826628881893,71.396309438915,202.750490121702));
#30467=CARTESIAN_POINT('',(72.7613803090644,69.2262674964981,202.750490121702));
#30468=CARTESIAN_POINT('',(72.7737552404501,69.2463619539781,202.750490121702));
#30469=CARTESIAN_POINT('Origin',(77.215862801455,80.368869783441,202.750490121702));
#30470=CARTESIAN_POINT('Origin',(72.7737552404501,69.2463619539781,192.750490121702));
#30471=CARTESIAN_POINT('',(72.7737552404501,69.2463619539781,196.17168857984));
#30472=CARTESIAN_POINT('',(71.699254778236,67.5015842920036,197.750490121702));
#30473=CARTESIAN_POINT('Ctrl Pts',(72.7737552404501,69.2463619539781,196.17168857984));
#30474=CARTESIAN_POINT('Ctrl Pts',(72.2783498325298,68.4419208953121,196.898024398673));
#30475=CARTESIAN_POINT('Ctrl Pts',(71.699254778236,67.5015842920036,197.750490121702));
#30476=CARTESIAN_POINT('',(71.699254778236,67.5015842920036,202.750490121702));
#30477=CARTESIAN_POINT('',(71.699254778236,67.5015842920036,202.950490121702));
#30478=CARTESIAN_POINT('',(72.7737552404501,69.2463619539781,202.750490121702));
#30479=CARTESIAN_POINT('',(72.7737552404501,69.2463619539781,192.750490121702));
#30480=CARTESIAN_POINT('Origin',(69.2826628881893,71.396309438915,192.750490121702));
#30481=CARTESIAN_POINT('',(69.2826628881893,71.396309438915,196.17168857984));
#30482=CARTESIAN_POINT('Ctrl Pts',(69.2826628881894,71.396309438915,196.17168857984));
#30483=CARTESIAN_POINT('Ctrl Pts',(71.0282090643197,70.3213356964465,195.897880393518));
#30484=CARTESIAN_POINT('Ctrl Pts',(72.7737552404501,69.2463619539781,196.17168857984));
#30485=CARTESIAN_POINT('',(69.2826628881893,71.396309438915,192.750490121702));
#30486=CARTESIAN_POINT('Origin',(69.2826628881893,71.396309438915,192.750490121702));
#30487=CARTESIAN_POINT('',(68.2081624259752,69.6515317769404,197.750490121702));
#30488=CARTESIAN_POINT('Ctrl Pts',(68.2081624259752,69.6515317769404,197.750490121702));
#30489=CARTESIAN_POINT('Ctrl Pts',(68.7872574802692,70.5918683802492,196.898024398673));
#30490=CARTESIAN_POINT('Ctrl Pts',(69.2826628881893,71.396309438915,196.17168857984));
#30491=CARTESIAN_POINT('',(68.2081624259752,69.6515317769404,202.750490121702));
#30492=CARTESIAN_POINT('',(69.2826628881893,71.396309438915,202.750490121702));
#30493=CARTESIAN_POINT('',(68.2081624259752,69.6515317769404,202.950490121702));
#30494=CARTESIAN_POINT('Origin',(77.215862801455,80.368869783441,202.750490121702));
#30495=CARTESIAN_POINT('',(68.2433024569292,88.3020696967067,202.750490121702));
#30496=CARTESIAN_POINT('',(68.223207999449,88.3144446280925,202.750490121702));
#30497=CARTESIAN_POINT('',(68.2433024569292,88.3020696967067,202.750490121702));
#30498=CARTESIAN_POINT('',(66.0933549719922,84.810977344446,202.750490121702));
#30499=CARTESIAN_POINT('',(68.2433024569292,88.3020696967067,202.750490121702));
#30500=CARTESIAN_POINT('',(66.0732605145121,84.8233522758317,202.750490121702));
#30501=CARTESIAN_POINT('',(66.0933549719922,84.810977344446,202.750490121702));
#30502=CARTESIAN_POINT('',(66.9980315265455,86.6613990076467,202.750490121702));
#30503=CARTESIAN_POINT('Origin',(77.215862801455,80.368869783441,202.750490121702));
#30504=CARTESIAN_POINT('Origin',(77.215862801455,80.368869783441,202.750490121702));
#30505=CARTESIAN_POINT('Origin',(66.0933549719922,84.810977344446,192.750490121702));
#30506=CARTESIAN_POINT('',(66.0933549719922,84.810977344446,196.17168857984));
#30507=CARTESIAN_POINT('',(64.3485773100176,85.8854778066601,197.750490121702));
#30508=CARTESIAN_POINT('Ctrl Pts',(66.0933549719923,84.810977344446,196.17168857984));
#30509=CARTESIAN_POINT('Ctrl Pts',(65.2889139133265,85.3063827523661,196.898024398673));
#30510=CARTESIAN_POINT('Ctrl Pts',(64.3485773100176,85.8854778066601,197.750490121702));
#30511=CARTESIAN_POINT('',(64.3485773100176,85.8854778066601,202.750490121702));
#30512=CARTESIAN_POINT('',(64.3485773100176,85.8854778066601,202.950490121702));
#30513=CARTESIAN_POINT('',(66.0933549719922,84.810977344446,202.750490121702));
#30514=CARTESIAN_POINT('',(66.0933549719922,84.810977344446,192.750490121702));
#30515=CARTESIAN_POINT('Origin',(68.2433024569292,88.3020696967067,192.750490121702));
#30516=CARTESIAN_POINT('',(68.2433024569292,88.3020696967067,196.17168857984));
#30517=CARTESIAN_POINT('',(67.1683287144608,86.5565235205765,196.033766787946));
#30518=CARTESIAN_POINT('Ctrl Pts',(68.2433024569291,88.3020696967066,196.17168857984));
#30519=CARTESIAN_POINT('Ctrl Pts',(67.7018200900497,87.42280870864,196.033766787946));
#30520=CARTESIAN_POINT('Ctrl Pts',(67.1683287144608,86.5565235205765,196.033766787946));
#30521=CARTESIAN_POINT('Ctrl Pts',(67.1683287144608,86.5565235205765,196.033766787946));
#30522=CARTESIAN_POINT('Ctrl Pts',(66.6348373388718,85.6902383325128,196.033766787946));
#30523=CARTESIAN_POINT('Ctrl Pts',(66.0933549719923,84.810977344446,196.17168857984));
#30524=CARTESIAN_POINT('',(68.2433024569292,88.3020696967067,192.750490121702));
#30525=CARTESIAN_POINT('Origin',(68.2433024569292,88.3020696967067,192.750490121702));
#30526=CARTESIAN_POINT('',(66.4985247949545,89.3765701589209,197.750490121702));
#30527=CARTESIAN_POINT('Ctrl Pts',(66.4985247949545,89.3765701589209,197.750490121702));
#30528=CARTESIAN_POINT('Ctrl Pts',(67.4388613982627,88.7974751046273,196.898024398674));
#30529=CARTESIAN_POINT('Ctrl Pts',(68.2433024569292,88.3020696967067,196.17168857984));
#30530=CARTESIAN_POINT('',(66.4985247949545,89.3765701589209,202.750490121702));
#30531=CARTESIAN_POINT('',(68.2433024569292,88.3020696967067,202.750490121702));
#30532=CARTESIAN_POINT('',(66.4985247949545,89.3765701589209,202.950490121702));
#30533=CARTESIAN_POINT('Origin',(77.215862801455,80.368869783441,202.950490121702));
#30534=CARTESIAN_POINT('Origin',(77.215862801455,80.368869783441,202.750490121702));
#30535=CARTESIAN_POINT('Origin',(77.215862801455,80.368869783441,197.750490121702));
#30536=CARTESIAN_POINT('Origin',(83.5083920256607,90.5867010583505,202.750490121702));
#30537=CARTESIAN_POINT('Origin',(77.215862801455,80.368869783441,202.750490121702));
#30538=CARTESIAN_POINT('Origin',(77.215862801455,80.368869783441,202.950490121702));
#30539=CARTESIAN_POINT('',(66.9980315265455,86.6613990076467,202.950490121702));
#30540=CARTESIAN_POINT('Origin',(77.215862801455,80.368869783441,202.950490121702));
#30541=CARTESIAN_POINT('',(66.9980315265455,86.6613990076467,202.950490121702));
#30542=CARTESIAN_POINT('Origin',(77.215862801455,80.368869783441,202.750490121702));
#30543=CARTESIAN_POINT('Origin',(77.215862801455,80.368869783441,202.750490121702));
#30544=CARTESIAN_POINT('Origin',(77.215862801455,80.368869783441,202.750490121702));
#30545=CARTESIAN_POINT('Origin',(81.4633200277938,87.2659058940049,202.950490121702));
#30546=CARTESIAN_POINT('Ctrl Pts',(68.8559951920602,81.9059493368123,202.950490121702));
#30547=CARTESIAN_POINT('Ctrl Pts',(68.7642152247191,81.2289065497019,202.950490121702));
#30548=CARTESIAN_POINT('Ctrl Pts',(68.7558437672831,80.5431690260287,202.950490121702));
#30549=CARTESIAN_POINT('Ctrl Pts',(68.9037765039421,79.208383788559,202.950490121702));
#30550=CARTESIAN_POINT('Ctrl Pts',(69.0539008969734,78.5636087221873,202.950490121702));
#30551=CARTESIAN_POINT('Ctrl Pts',(69.5077654228198,77.3091162265887,202.950490121702));
#30552=CARTESIAN_POINT('Ctrl Pts',(69.8131562970982,76.7051358769036,202.950490121702));
#30553=CARTESIAN_POINT('Ctrl Pts',(70.3807100616133,75.8558168618057,202.950490121702));
#30554=CARTESIAN_POINT('Ctrl Pts',(70.5846181218229,75.5896281769766,202.950490121702));
#30555=CARTESIAN_POINT('Ctrl Pts',(71.0222837417832,75.0866685278261,202.950490121702));
#30556=CARTESIAN_POINT('Ctrl Pts',(71.2518555252683,74.8532966906131,202.950490121702));
#30557=CARTESIAN_POINT('Ctrl Pts',(71.4950332612282,74.6345773796944,202.950490121702));
#30558=CARTESIAN_POINT('Ctrl Pts',(80.1444697952855,87.9209066660103,202.950490121702));
#30559=CARTESIAN_POINT('Ctrl Pts',(79.3727964197385,88.2659773938407,202.950490121702));
#30560=CARTESIAN_POINT('Ctrl Pts',(78.6856433791405,88.4271476868973,202.950490121702));
#30561=CARTESIAN_POINT('Ctrl Pts',(77.5319949492831,88.6233670935503,202.950490121702));
#30562=CARTESIAN_POINT('Ctrl Pts',(76.8660965396909,88.6557827059197,202.950490121702));
#30563=CARTESIAN_POINT('Ctrl Pts',(75.5487931964297,88.5618133194148,202.950490121702));
#30564=CARTESIAN_POINT('Ctrl Pts',(74.9019787775752,88.4376650266567,202.950490121702));
#30565=CARTESIAN_POINT('Ctrl Pts',(73.6122724742245,88.0273485574021,202.950490121702));
#30566=CARTESIAN_POINT('Ctrl Pts',(72.9824334762108,87.7347023571041,202.950490121702));
#30567=CARTESIAN_POINT('Ctrl Pts',(72.3914232244021,87.3670683207338,202.950490121702));
#30568=CARTESIAN_POINT('Origin',(77.215862801455,80.368869783441,202.950490121702));
#30569=CARTESIAN_POINT('',(70.3188266908911,84.6163270097798,195.150490121702));
#30570=CARTESIAN_POINT('Origin',(77.215862801455,80.368869783441,195.150490121702));
#30571=CARTESIAN_POINT('',(70.3188266908911,84.6163270097798,196.));
#30572=CARTESIAN_POINT('',(70.3188266908911,84.6163270097798,202.950490121702));
#30573=CARTESIAN_POINT('Origin',(77.215862801455,80.368869783441,196.));
#30574=CARTESIAN_POINT('Origin',(77.215862801455,80.368869783441,199.24883868241));
#30575=CARTESIAN_POINT('',(67.6632584598299,86.2517269543706,195.58019743297));
#30576=CARTESIAN_POINT('Origin',(77.215862801455,80.368869783441,195.58019743297));
#30577=CARTESIAN_POINT('Origin',(69.4466522947436,85.1534451837547,199.24883868241));
#30578=CARTESIAN_POINT('Origin',(77.215862801455,80.368869783441,197.750490121702));
#30579=CARTESIAN_POINT('Origin',(77.215862801455,80.368869783441,197.750490121702));
#30580=CARTESIAN_POINT('Origin',(77.215862801455,80.368869783441,197.750490121702));
#30581=CARTESIAN_POINT('',(65.295059647394,87.7101538783476,197.750490121702));
#30582=CARTESIAN_POINT('Origin',(77.215862801455,80.368869783441,197.750490121702));
#30583=CARTESIAN_POINT('Origin',(77.215862801455,80.368869783441,202.950490121702));
#30584=CARTESIAN_POINT('Origin',(77.215862801455,80.368869783441,202.750490121702));
#30585=CARTESIAN_POINT('Origin',(77.215862801455,80.368869783441,202.950490121702));
#30586=CARTESIAN_POINT('Origin',(77.215862801455,80.368869783441,202.750490121702));
#30587=CARTESIAN_POINT('Origin',(77.215862801455,80.368869783441,202.950490121702));
#30588=CARTESIAN_POINT('Origin',(77.215862801455,80.368869783441,202.750490121702));
#30589=CARTESIAN_POINT('Origin',(83.5083920256607,90.5867010583505,202.750490121702));
#30590=CARTESIAN_POINT('Origin',(83.5083920256607,90.5867010583505,202.750490121702));
#30591=CARTESIAN_POINT('Origin',(83.5083920256607,90.5867010583505,202.750490121702));
#30592=CARTESIAN_POINT('Ctrl Pts',(75.2070279073809,72.1096563878274,197.312500795565));
#30593=CARTESIAN_POINT('Ctrl Pts',(78.6281061103777,71.2775697301335,197.406250795565));
#30594=CARTESIAN_POINT('Ctrl Pts',(81.6355478248763,73.1082632082519,197.500000795565));
#30595=CARTESIAN_POINT('Ctrl Pts',(84.6429895393749,74.9389566863702,197.593750795565));
#30596=CARTESIAN_POINT('Ctrl Pts',(85.4750761970687,78.360034889367,197.687500795565));
#30597=CARTESIAN_POINT('Ctrl Pts',(86.3071628547625,81.7811130923637,197.781250795565));
#30598=CARTESIAN_POINT('Ctrl Pts',(84.4764693766442,84.7885548068623,197.875000795565));
#30599=CARTESIAN_POINT('Ctrl Pts',(82.6457758985258,87.7959965213609,197.968750795565));
#30600=CARTESIAN_POINT('Ctrl Pts',(79.2246976955291,88.6280831790547,198.062500795565));
#30601=CARTESIAN_POINT('Ctrl Pts',(75.8036194925323,89.4601698367485,198.156250795565));
#30602=CARTESIAN_POINT('Ctrl Pts',(72.7961777780337,87.6294763586302,198.250000795565));
#30603=CARTESIAN_POINT('Ctrl Pts',(69.7887360635351,85.7987828805119,198.343750795565));
#30604=CARTESIAN_POINT('Ctrl Pts',(68.9566494058413,82.3777046775151,198.437500795565));
#30605=CARTESIAN_POINT('Ctrl Pts',(68.1245627481475,78.9566264745184,198.531250795565));
#30606=CARTESIAN_POINT('Ctrl Pts',(69.9552562262659,75.9491847600198,198.625000795565));
#30607=CARTESIAN_POINT('Ctrl Pts',(71.7859497043842,72.9417430455211,198.718750795565));
#30608=CARTESIAN_POINT('Ctrl Pts',(75.2070279073809,72.1096563878274,198.812500795565));
#30609=CARTESIAN_POINT('Ctrl Pts',(78.6281061103777,71.2775697301335,198.906250795565));
#30610=CARTESIAN_POINT('Ctrl Pts',(81.6355478248763,73.1082632082519,199.000000795565));
#30611=CARTESIAN_POINT('Ctrl Pts',(84.6429895393749,74.9389566863702,199.093750795565));
#30612=CARTESIAN_POINT('Ctrl Pts',(85.4750761970687,78.360034889367,199.187500795565));
#30613=CARTESIAN_POINT('Ctrl Pts',(86.3071628547625,81.7811130923637,199.281250795565));
#30614=CARTESIAN_POINT('Ctrl Pts',(84.4764693766442,84.7885548068623,199.375000795565));
#30615=CARTESIAN_POINT('Ctrl Pts',(82.6457758985258,87.7959965213609,199.468750795565));
#30616=CARTESIAN_POINT('Ctrl Pts',(79.2246976955291,88.6280831790547,199.562500795565));
#30617=CARTESIAN_POINT('Ctrl Pts',(75.8036194925323,89.4601698367485,199.656250795565));
#30618=CARTESIAN_POINT('Ctrl Pts',(72.7961777780337,87.6294763586302,199.750000795565));
#30619=CARTESIAN_POINT('Ctrl Pts',(69.7887360635351,85.7987828805119,199.843750795565));
#30620=CARTESIAN_POINT('Ctrl Pts',(68.9566494058413,82.3777046775151,199.937500795565));
#30621=CARTESIAN_POINT('Ctrl Pts',(68.1245627481475,78.9566264745184,200.031250795565));
#30622=CARTESIAN_POINT('Ctrl Pts',(69.9552562262659,75.9491847600198,200.125000795565));
#30623=CARTESIAN_POINT('Ctrl Pts',(71.7859497043842,72.9417430455211,200.218750795565));
#30624=CARTESIAN_POINT('Ctrl Pts',(75.2070279073809,72.1096563878274,200.312500795565));
#30625=CARTESIAN_POINT('Ctrl Pts',(78.6281061103777,71.2775697301335,200.406250795565));
#30626=CARTESIAN_POINT('Ctrl Pts',(81.6355478248763,73.1082632082519,200.500000795565));
#30627=CARTESIAN_POINT('Ctrl Pts',(84.6429895393749,74.9389566863702,200.593750795565));
#30628=CARTESIAN_POINT('Ctrl Pts',(85.4750761970687,78.360034889367,200.687500795565));
#30629=CARTESIAN_POINT('Ctrl Pts',(86.3071628547625,81.7811130923637,200.781250795565));
#30630=CARTESIAN_POINT('Ctrl Pts',(84.4764693766442,84.7885548068623,200.875000795565));
#30631=CARTESIAN_POINT('Ctrl Pts',(82.6457758985258,87.7959965213609,200.968750795565));
#30632=CARTESIAN_POINT('Ctrl Pts',(79.2246976955291,88.6280831790547,201.062500795565));
#30633=CARTESIAN_POINT('Ctrl Pts',(75.8036194925323,89.4601698367485,201.156250795565));
#30634=CARTESIAN_POINT('Ctrl Pts',(72.7961777780337,87.6294763586302,201.250000795565));
#30635=CARTESIAN_POINT('Ctrl Pts',(69.7887360635351,85.7987828805119,201.343750795565));
#30636=CARTESIAN_POINT('Ctrl Pts',(68.9566494058413,82.3777046775151,201.437500795565));
#30637=CARTESIAN_POINT('Ctrl Pts',(68.1245627481475,78.9566264745183,201.531250795565));
#30638=CARTESIAN_POINT('Ctrl Pts',(69.9552562262659,75.9491847600198,201.625000795565));
#30639=CARTESIAN_POINT('Ctrl Pts',(71.7859497043842,72.9417430455211,201.718750795565));
#30640=CARTESIAN_POINT('Ctrl Pts',(75.2070279073809,72.1096563878273,201.812500795565));
#30641=CARTESIAN_POINT('Ctrl Pts',(78.6281061103777,71.2775697301335,201.906250795565));
#30642=CARTESIAN_POINT('Ctrl Pts',(81.6355478248763,73.1082632082519,202.000000795565));
#30643=CARTESIAN_POINT('Ctrl Pts',(84.6429895393749,74.9389566863702,202.093750795565));
#30644=CARTESIAN_POINT('Ctrl Pts',(85.4750761970687,78.360034889367,202.187500795565));
#30645=CARTESIAN_POINT('Ctrl Pts',(86.3071628547625,81.7811130923637,202.281250795565));
#30646=CARTESIAN_POINT('Ctrl Pts',(84.4764693766442,84.7885548068623,202.375000795565));
#30647=CARTESIAN_POINT('Ctrl Pts',(82.6457758985258,87.7959965213609,202.468750795565));
#30648=CARTESIAN_POINT('Ctrl Pts',(79.2246976955291,88.6280831790547,202.562500795565));
#30649=CARTESIAN_POINT('Ctrl Pts',(75.8036194925323,89.4601698367485,202.656250795565));
#30650=CARTESIAN_POINT('Ctrl Pts',(72.7961777780337,87.6294763586302,202.750000795565));
#30651=CARTESIAN_POINT('Ctrl Pts',(69.7887360635351,85.7987828805119,202.843750795565));
#30652=CARTESIAN_POINT('Ctrl Pts',(68.9566494058413,82.3777046775151,202.937500795565));
#30653=CARTESIAN_POINT('Ctrl Pts',(68.1245627481475,78.9566264745183,203.031250795565));
#30654=CARTESIAN_POINT('Ctrl Pts',(69.9552562262658,75.9491847600198,203.125000795565));
#30655=CARTESIAN_POINT('Ctrl Pts',(71.7859497043842,72.9417430455211,203.218750795565));
#30656=CARTESIAN_POINT('Ctrl Pts',(75.2070279073809,72.1096563878273,203.312500795565));
#30657=CARTESIAN_POINT('Ctrl Pts',(78.6281061103777,71.2775697301335,203.406250795565));
#30658=CARTESIAN_POINT('Ctrl Pts',(81.6355478248763,73.1082632082519,203.500000795565));
#30659=CARTESIAN_POINT('Ctrl Pts',(84.6429895393749,74.9389566863702,203.593750795565));
#30660=CARTESIAN_POINT('Ctrl Pts',(85.4750761970687,78.360034889367,203.687500795565));
#30661=CARTESIAN_POINT('Ctrl Pts',(86.3071628547625,81.7811130923637,203.781250795565));
#30662=CARTESIAN_POINT('Ctrl Pts',(84.4764693766442,84.7885548068623,203.875000795565));
#30663=CARTESIAN_POINT('Ctrl Pts',(82.6457758985258,87.7959965213609,203.968750795565));
#30664=CARTESIAN_POINT('Ctrl Pts',(79.2246976955291,88.6280831790547,204.062500795565));
#30665=CARTESIAN_POINT('Ctrl Pts',(75.8036194925323,89.4601698367485,204.156250795565));
#30666=CARTESIAN_POINT('Ctrl Pts',(72.7961777780337,87.6294763586302,204.250000795565));
#30667=CARTESIAN_POINT('Ctrl Pts',(69.7887360635351,85.7987828805118,204.343750795565));
#30668=CARTESIAN_POINT('Ctrl Pts',(68.9566494058413,82.3777046775151,204.437500795565));
#30669=CARTESIAN_POINT('Ctrl Pts',(68.1245627481475,78.9566264745183,204.531250795565));
#30670=CARTESIAN_POINT('Ctrl Pts',(69.9552562262658,75.9491847600198,204.625000795565));
#30671=CARTESIAN_POINT('Ctrl Pts',(71.7859497043842,72.9417430455211,204.718750795565));
#30672=CARTESIAN_POINT('Ctrl Pts',(75.2070279073809,72.1096563878273,204.812500795565));
#30673=CARTESIAN_POINT('Ctrl Pts',(78.6281061103777,71.2775697301335,204.906250795565));
#30674=CARTESIAN_POINT('Ctrl Pts',(81.6355478248763,73.1082632082519,205.000000795565));
#30675=CARTESIAN_POINT('Ctrl Pts',(84.6429895393749,74.9389566863702,205.093750795565));
#30676=CARTESIAN_POINT('Ctrl Pts',(85.4750761970687,78.360034889367,205.187500795565));
#30677=CARTESIAN_POINT('Ctrl Pts',(86.3071628547625,81.7811130923637,205.281250795565));
#30678=CARTESIAN_POINT('Ctrl Pts',(84.4764693766442,84.7885548068623,205.375000795565));
#30679=CARTESIAN_POINT('Ctrl Pts',(82.6457758985258,87.7959965213609,205.468750795565));
#30680=CARTESIAN_POINT('Ctrl Pts',(79.2246976955291,88.6280831790547,205.562500795565));
#30681=CARTESIAN_POINT('Ctrl Pts',(75.8036194925323,89.4601698367485,205.656250795565));
#30682=CARTESIAN_POINT('Ctrl Pts',(72.7961777780337,87.6294763586302,205.750000795565));
#30683=CARTESIAN_POINT('Ctrl Pts',(69.7887360635351,85.7987828805118,205.843750795565));
#30684=CARTESIAN_POINT('Ctrl Pts',(68.9566494058413,82.3777046775151,205.937500795565));
#30685=CARTESIAN_POINT('Ctrl Pts',(68.1245627481475,78.9566264745183,206.031250795565));
#30686=CARTESIAN_POINT('Ctrl Pts',(69.9552562262658,75.9491847600198,206.125000795565));
#30687=CARTESIAN_POINT('Ctrl Pts',(71.7859497043842,72.9417430455211,206.218750795565));
#30688=CARTESIAN_POINT('Ctrl Pts',(75.2070279073809,72.1096563878273,206.312500795565));
#30689=CARTESIAN_POINT('Ctrl Pts',(78.6281061103777,71.2775697301335,206.406250795565));
#30690=CARTESIAN_POINT('Ctrl Pts',(81.6355478248763,73.1082632082519,206.500000795565));
#30691=CARTESIAN_POINT('Ctrl Pts',(84.6429895393749,74.9389566863702,206.593750795565));
#30692=CARTESIAN_POINT('Ctrl Pts',(85.4750761970687,78.3600348893669,206.687500795565));
#30693=CARTESIAN_POINT('Ctrl Pts',(86.3071628547625,81.7811130923637,206.781250795565));
#30694=CARTESIAN_POINT('Ctrl Pts',(84.4764693766442,84.7885548068623,206.875000795565));
#30695=CARTESIAN_POINT('Ctrl Pts',(82.6457758985258,87.7959965213609,206.968750795565));
#30696=CARTESIAN_POINT('Ctrl Pts',(79.2246976955291,88.6280831790547,207.062500795565));
#30697=CARTESIAN_POINT('Ctrl Pts',(75.8036194925323,89.4601698367485,207.156250795565));
#30698=CARTESIAN_POINT('Ctrl Pts',(72.7961777780337,87.6294763586302,207.250000795565));
#30699=CARTESIAN_POINT('Ctrl Pts',(69.7887360635351,85.7987828805118,207.343750795565));
#30700=CARTESIAN_POINT('Ctrl Pts',(68.9566494058413,82.3777046775151,207.437500795565));
#30701=CARTESIAN_POINT('Ctrl Pts',(68.1245627481475,78.9566264745183,207.531250795565));
#30702=CARTESIAN_POINT('Ctrl Pts',(69.9552562262658,75.9491847600198,207.625000795565));
#30703=CARTESIAN_POINT('Ctrl Pts',(71.7859497043842,72.9417430455211,207.718750795565));
#30704=CARTESIAN_POINT('Ctrl Pts',(75.2070279073809,72.1096563878273,207.812500795565));
#30705=CARTESIAN_POINT('Ctrl Pts',(78.6281061103777,71.2775697301335,207.906250795565));
#30706=CARTESIAN_POINT('Ctrl Pts',(81.6355478248763,73.1082632082518,208.000000795565));
#30707=CARTESIAN_POINT('Ctrl Pts',(84.6429895393749,74.9389566863702,208.093750795565));
#30708=CARTESIAN_POINT('Ctrl Pts',(85.4750761970687,78.3600348893669,208.187500795565));
#30709=CARTESIAN_POINT('Ctrl Pts',(86.3071628547625,81.7811130923637,208.281250795565));
#30710=CARTESIAN_POINT('Ctrl Pts',(84.4764693766442,84.7885548068623,208.375000795565));
#30711=CARTESIAN_POINT('Ctrl Pts',(82.6457758985258,87.7959965213609,208.468750795565));
#30712=CARTESIAN_POINT('Ctrl Pts',(79.2246976955291,88.6280831790547,208.562500795565));
#30713=CARTESIAN_POINT('Ctrl Pts',(75.8036194925323,89.4601698367485,208.656250795565));
#30714=CARTESIAN_POINT('Ctrl Pts',(72.7961777780337,87.6294763586302,208.750000795565));
#30715=CARTESIAN_POINT('Ctrl Pts',(69.7887360635351,85.7987828805118,208.843750795565));
#30716=CARTESIAN_POINT('Ctrl Pts',(68.9566494058413,82.3777046775151,208.937500795565));
#30717=CARTESIAN_POINT('Ctrl Pts',(68.1245627481475,78.9566264745183,209.031250795565));
#30718=CARTESIAN_POINT('Ctrl Pts',(69.9552562262658,75.9491847600198,209.125000795565));
#30719=CARTESIAN_POINT('Ctrl Pts',(71.7859497043842,72.9417430455211,209.218750795565));
#30720=CARTESIAN_POINT('Ctrl Pts',(75.2070279073809,72.1096563878273,209.312500795565));
#30721=CARTESIAN_POINT('Ctrl Pts',(75.3989071052151,72.8985570813421,196.843749997952));
#30722=CARTESIAN_POINT('Ctrl Pts',(78.4932119415925,72.1459493897285,196.937499997952));
#30723=CARTESIAN_POINT('Ctrl Pts',(81.2133898767664,73.8017793202762,197.031249997952));
#30724=CARTESIAN_POINT('Ctrl Pts',(83.9335678119403,75.4576092508238,197.124999997952));
#30725=CARTESIAN_POINT('Ctrl Pts',(84.6861755035539,78.5519140872012,197.218749997952));
#30726=CARTESIAN_POINT('Ctrl Pts',(85.4387831951675,81.6462189235785,197.312499997952));
#30727=CARTESIAN_POINT('Ctrl Pts',(83.7829532646199,84.3663968587524,197.406249997952));
#30728=CARTESIAN_POINT('Ctrl Pts',(82.1271233340723,87.0865747939263,197.499999997952));
#30729=CARTESIAN_POINT('Ctrl Pts',(79.0328184976949,87.83918248554,197.593749997952));
#30730=CARTESIAN_POINT('Ctrl Pts',(75.9385136613175,88.5917901771536,197.687499997952));
#30731=CARTESIAN_POINT('Ctrl Pts',(73.2183357261436,86.9359602466059,197.781249997952));
#30732=CARTESIAN_POINT('Ctrl Pts',(70.4981577909697,85.2801303160583,197.874999997952));
#30733=CARTESIAN_POINT('Ctrl Pts',(69.7455500993561,82.1858254796809,197.968749997952));
#30734=CARTESIAN_POINT('Ctrl Pts',(68.9929424077425,79.0915206433035,198.062499997952));
#30735=CARTESIAN_POINT('Ctrl Pts',(70.6487723382901,76.3713427081296,198.156249997952));
#30736=CARTESIAN_POINT('Ctrl Pts',(72.3046022688378,73.6511647729557,198.249999997952));
#30737=CARTESIAN_POINT('Ctrl Pts',(75.3989071052151,72.8985570813421,198.343749997952));
#30738=CARTESIAN_POINT('Ctrl Pts',(78.4932119415925,72.1459493897285,198.437499997952));
#30739=CARTESIAN_POINT('Ctrl Pts',(81.2133898767664,73.8017793202762,198.531249997952));
#30740=CARTESIAN_POINT('Ctrl Pts',(83.9335678119403,75.4576092508238,198.624999997952));
#30741=CARTESIAN_POINT('Ctrl Pts',(84.6861755035539,78.5519140872012,198.718749997952));
#30742=CARTESIAN_POINT('Ctrl Pts',(85.4387831951675,81.6462189235785,198.812499997952));
#30743=CARTESIAN_POINT('Ctrl Pts',(83.7829532646199,84.3663968587524,198.906249997952));
#30744=CARTESIAN_POINT('Ctrl Pts',(82.1271233340723,87.0865747939263,198.999999997952));
#30745=CARTESIAN_POINT('Ctrl Pts',(79.0328184976949,87.8391824855399,199.093749997952));
#30746=CARTESIAN_POINT('Ctrl Pts',(75.9385136613175,88.5917901771536,199.187499997952));
#30747=CARTESIAN_POINT('Ctrl Pts',(73.2183357261436,86.9359602466059,199.281249997952));
#30748=CARTESIAN_POINT('Ctrl Pts',(70.4981577909697,85.2801303160583,199.374999997952));
#30749=CARTESIAN_POINT('Ctrl Pts',(69.7455500993561,82.1858254796809,199.468749997952));
#30750=CARTESIAN_POINT('Ctrl Pts',(68.9929424077425,79.0915206433035,199.562499997952));
#30751=CARTESIAN_POINT('Ctrl Pts',(70.6487723382901,76.3713427081296,199.656249997952));
#30752=CARTESIAN_POINT('Ctrl Pts',(72.3046022688378,73.6511647729557,199.749999997952));
#30753=CARTESIAN_POINT('Ctrl Pts',(75.3989071052151,72.8985570813421,199.843749997952));
#30754=CARTESIAN_POINT('Ctrl Pts',(78.4932119415925,72.1459493897285,199.937499997952));
#30755=CARTESIAN_POINT('Ctrl Pts',(81.2133898767664,73.8017793202761,200.031249997952));
#30756=CARTESIAN_POINT('Ctrl Pts',(83.9335678119403,75.4576092508238,200.124999997952));
#30757=CARTESIAN_POINT('Ctrl Pts',(84.6861755035539,78.5519140872012,200.218749997952));
#30758=CARTESIAN_POINT('Ctrl Pts',(85.4387831951675,81.6462189235785,200.312499997952));
#30759=CARTESIAN_POINT('Ctrl Pts',(83.7829532646199,84.3663968587524,200.406249997952));
#30760=CARTESIAN_POINT('Ctrl Pts',(82.1271233340723,87.0865747939263,200.499999997952));
#30761=CARTESIAN_POINT('Ctrl Pts',(79.0328184976949,87.8391824855399,200.593749997952));
#30762=CARTESIAN_POINT('Ctrl Pts',(75.9385136613175,88.5917901771536,200.687499997952));
#30763=CARTESIAN_POINT('Ctrl Pts',(73.2183357261436,86.9359602466059,200.781249997952));
#30764=CARTESIAN_POINT('Ctrl Pts',(70.4981577909697,85.2801303160583,200.874999997952));
#30765=CARTESIAN_POINT('Ctrl Pts',(69.7455500993561,82.1858254796809,200.968749997952));
#30766=CARTESIAN_POINT('Ctrl Pts',(68.9929424077425,79.0915206433035,201.062499997952));
#30767=CARTESIAN_POINT('Ctrl Pts',(70.6487723382901,76.3713427081296,201.156249997952));
#30768=CARTESIAN_POINT('Ctrl Pts',(72.3046022688378,73.6511647729557,201.249999997952));
#30769=CARTESIAN_POINT('Ctrl Pts',(75.3989071052151,72.8985570813421,201.343749997952));
#30770=CARTESIAN_POINT('Ctrl Pts',(78.4932119415925,72.1459493897285,201.437499997952));
#30771=CARTESIAN_POINT('Ctrl Pts',(81.2133898767664,73.8017793202761,201.531249997952));
#30772=CARTESIAN_POINT('Ctrl Pts',(83.9335678119403,75.4576092508238,201.624999997952));
#30773=CARTESIAN_POINT('Ctrl Pts',(84.6861755035539,78.5519140872011,201.718749997952));
#30774=CARTESIAN_POINT('Ctrl Pts',(85.4387831951675,81.6462189235785,201.812499997952));
#30775=CARTESIAN_POINT('Ctrl Pts',(83.7829532646199,84.3663968587524,201.906249997952));
#30776=CARTESIAN_POINT('Ctrl Pts',(82.1271233340723,87.0865747939263,201.999999997952));
#30777=CARTESIAN_POINT('Ctrl Pts',(79.0328184976949,87.8391824855399,202.093749997952));
#30778=CARTESIAN_POINT('Ctrl Pts',(75.9385136613175,88.5917901771535,202.187499997952));
#30779=CARTESIAN_POINT('Ctrl Pts',(73.2183357261436,86.9359602466059,202.281249997952));
#30780=CARTESIAN_POINT('Ctrl Pts',(70.4981577909697,85.2801303160583,202.374999997952));
#30781=CARTESIAN_POINT('Ctrl Pts',(69.7455500993561,82.1858254796809,202.468749997952));
#30782=CARTESIAN_POINT('Ctrl Pts',(68.9929424077425,79.0915206433035,202.562499997952));
#30783=CARTESIAN_POINT('Ctrl Pts',(70.6487723382901,76.3713427081296,202.656249997952));
#30784=CARTESIAN_POINT('Ctrl Pts',(72.3046022688378,73.6511647729557,202.749999997952));
#30785=CARTESIAN_POINT('Ctrl Pts',(75.3989071052151,72.8985570813421,202.843749997952));
#30786=CARTESIAN_POINT('Ctrl Pts',(78.4932119415925,72.1459493897285,202.937499997952));
#30787=CARTESIAN_POINT('Ctrl Pts',(81.2133898767664,73.8017793202761,203.031249997952));
#30788=CARTESIAN_POINT('Ctrl Pts',(83.9335678119403,75.4576092508238,203.124999997952));
#30789=CARTESIAN_POINT('Ctrl Pts',(84.6861755035539,78.5519140872011,203.218749997952));
#30790=CARTESIAN_POINT('Ctrl Pts',(85.4387831951675,81.6462189235785,203.312499997952));
#30791=CARTESIAN_POINT('Ctrl Pts',(83.7829532646199,84.3663968587524,203.406249997952));
#30792=CARTESIAN_POINT('Ctrl Pts',(82.1271233340723,87.0865747939263,203.499999997952));
#30793=CARTESIAN_POINT('Ctrl Pts',(79.0328184976949,87.8391824855399,203.593749997952));
#30794=CARTESIAN_POINT('Ctrl Pts',(75.9385136613175,88.5917901771535,203.687499997952));
#30795=CARTESIAN_POINT('Ctrl Pts',(73.2183357261436,86.9359602466059,203.781249997952));
#30796=CARTESIAN_POINT('Ctrl Pts',(70.4981577909697,85.2801303160583,203.874999997952));
#30797=CARTESIAN_POINT('Ctrl Pts',(69.7455500993561,82.1858254796809,203.968749997952));
#30798=CARTESIAN_POINT('Ctrl Pts',(68.9929424077425,79.0915206433035,204.062499997952));
#30799=CARTESIAN_POINT('Ctrl Pts',(70.6487723382901,76.3713427081296,204.156249997952));
#30800=CARTESIAN_POINT('Ctrl Pts',(72.3046022688378,73.6511647729557,204.249999997952));
#30801=CARTESIAN_POINT('Ctrl Pts',(75.3989071052151,72.8985570813421,204.343749997952));
#30802=CARTESIAN_POINT('Ctrl Pts',(78.4932119415925,72.1459493897285,204.437499997952));
#30803=CARTESIAN_POINT('Ctrl Pts',(81.2133898767664,73.8017793202761,204.531249997952));
#30804=CARTESIAN_POINT('Ctrl Pts',(83.9335678119403,75.4576092508238,204.624999997952));
#30805=CARTESIAN_POINT('Ctrl Pts',(84.6861755035539,78.5519140872011,204.718749997952));
#30806=CARTESIAN_POINT('Ctrl Pts',(85.4387831951675,81.6462189235785,204.812499997952));
#30807=CARTESIAN_POINT('Ctrl Pts',(83.7829532646199,84.3663968587524,204.906249997952));
#30808=CARTESIAN_POINT('Ctrl Pts',(82.1271233340722,87.0865747939263,204.999999997952));
#30809=CARTESIAN_POINT('Ctrl Pts',(79.0328184976949,87.8391824855399,205.093749997952));
#30810=CARTESIAN_POINT('Ctrl Pts',(75.9385136613175,88.5917901771535,205.187499997952));
#30811=CARTESIAN_POINT('Ctrl Pts',(73.2183357261436,86.9359602466059,205.281249997952));
#30812=CARTESIAN_POINT('Ctrl Pts',(70.4981577909697,85.2801303160583,205.374999997952));
#30813=CARTESIAN_POINT('Ctrl Pts',(69.7455500993561,82.1858254796809,205.468749997952));
#30814=CARTESIAN_POINT('Ctrl Pts',(68.9929424077425,79.0915206433035,205.562499997952));
#30815=CARTESIAN_POINT('Ctrl Pts',(70.6487723382901,76.3713427081296,205.656249997952));
#30816=CARTESIAN_POINT('Ctrl Pts',(72.3046022688378,73.6511647729557,205.749999997952));
#30817=CARTESIAN_POINT('Ctrl Pts',(75.3989071052151,72.8985570813421,205.843749997952));
#30818=CARTESIAN_POINT('Ctrl Pts',(78.4932119415925,72.1459493897285,205.937499997952));
#30819=CARTESIAN_POINT('Ctrl Pts',(81.2133898767664,73.8017793202761,206.031249997952));
#30820=CARTESIAN_POINT('Ctrl Pts',(83.9335678119403,75.4576092508238,206.124999997952));
#30821=CARTESIAN_POINT('Ctrl Pts',(84.6861755035539,78.5519140872011,206.218749997952));
#30822=CARTESIAN_POINT('Ctrl Pts',(85.4387831951675,81.6462189235785,206.312499997952));
#30823=CARTESIAN_POINT('Ctrl Pts',(83.7829532646199,84.3663968587524,206.406249997952));
#30824=CARTESIAN_POINT('Ctrl Pts',(82.1271233340722,87.0865747939263,206.499999997952));
#30825=CARTESIAN_POINT('Ctrl Pts',(79.0328184976949,87.8391824855399,206.593749997952));
#30826=CARTESIAN_POINT('Ctrl Pts',(75.9385136613175,88.5917901771535,206.687499997952));
#30827=CARTESIAN_POINT('Ctrl Pts',(73.2183357261436,86.9359602466059,206.781249997952));
#30828=CARTESIAN_POINT('Ctrl Pts',(70.4981577909697,85.2801303160583,206.874999997952));
#30829=CARTESIAN_POINT('Ctrl Pts',(69.7455500993561,82.1858254796809,206.968749997952));
#30830=CARTESIAN_POINT('Ctrl Pts',(68.9929424077425,79.0915206433035,207.062499997952));
#30831=CARTESIAN_POINT('Ctrl Pts',(70.6487723382901,76.3713427081296,207.156249997952));
#30832=CARTESIAN_POINT('Ctrl Pts',(72.3046022688378,73.6511647729557,207.249999997952));
#30833=CARTESIAN_POINT('Ctrl Pts',(75.3989071052151,72.8985570813421,207.343749997952));
#30834=CARTESIAN_POINT('Ctrl Pts',(78.4932119415925,72.1459493897285,207.437499997952));
#30835=CARTESIAN_POINT('Ctrl Pts',(81.2133898767664,73.8017793202761,207.531249997952));
#30836=CARTESIAN_POINT('Ctrl Pts',(83.9335678119403,75.4576092508238,207.624999997952));
#30837=CARTESIAN_POINT('Ctrl Pts',(84.6861755035539,78.5519140872011,207.718749997952));
#30838=CARTESIAN_POINT('Ctrl Pts',(85.4387831951675,81.6462189235785,207.812499997952));
#30839=CARTESIAN_POINT('Ctrl Pts',(83.7829532646199,84.3663968587524,207.906249997952));
#30840=CARTESIAN_POINT('Ctrl Pts',(82.1271233340722,87.0865747939263,207.999999997952));
#30841=CARTESIAN_POINT('Ctrl Pts',(79.0328184976949,87.8391824855399,208.093749997952));
#30842=CARTESIAN_POINT('Ctrl Pts',(75.9385136613175,88.5917901771535,208.187499997952));
#30843=CARTESIAN_POINT('Ctrl Pts',(73.2183357261436,86.9359602466059,208.281249997952));
#30844=CARTESIAN_POINT('Ctrl Pts',(70.4981577909697,85.2801303160583,208.374999997952));
#30845=CARTESIAN_POINT('Ctrl Pts',(69.7455500993561,82.1858254796809,208.468749997952));
#30846=CARTESIAN_POINT('Ctrl Pts',(68.9929424077425,79.0915206433035,208.562499997952));
#30847=CARTESIAN_POINT('Ctrl Pts',(70.6487723382901,76.3713427081296,208.656249997952));
#30848=CARTESIAN_POINT('Ctrl Pts',(72.3046022688377,73.6511647729557,208.749999997952));
#30849=CARTESIAN_POINT('Ctrl Pts',(75.3989071052151,72.8985570813421,208.843749997952));
#30850=CARTESIAN_POINT('',(75.3989071052151,72.8985570813421,196.843749997952));
#30851=CARTESIAN_POINT('',(75.3029676699654,72.5041074074942,197.078124996927));
#30852=CARTESIAN_POINT('Ctrl Pts',(75.3989071052151,72.8985570813421,196.843749997952));
#30853=CARTESIAN_POINT('Ctrl Pts',(78.4932119415925,72.1459493897285,196.937499997952));
#30854=CARTESIAN_POINT('Ctrl Pts',(81.2133898767664,73.8017793202762,197.031249997952));
#30855=CARTESIAN_POINT('Ctrl Pts',(83.9335678119403,75.4576092508238,197.124999997952));
#30856=CARTESIAN_POINT('Ctrl Pts',(84.6861755035539,78.5519140872012,197.218749997952));
#30857=CARTESIAN_POINT('Ctrl Pts',(85.4387831951675,81.6462189235786,197.312499997952));
#30858=CARTESIAN_POINT('Ctrl Pts',(83.7829532646199,84.3663968587524,197.406249997952));
#30859=CARTESIAN_POINT('Ctrl Pts',(82.1271233340723,87.0865747939263,197.499999997952));
#30860=CARTESIAN_POINT('Ctrl Pts',(79.0328184976949,87.83918248554,197.593749997952));
#30861=CARTESIAN_POINT('',(75.2070282347158,72.1096577336463,209.312499995903));
#30862=CARTESIAN_POINT('',(75.3029676699654,72.5041074074942,209.078124996927));
#30863=CARTESIAN_POINT('',(81.6355472361212,73.1082644713496,208.));
#30864=CARTESIAN_POINT('Ctrl Pts',(81.6355472361214,73.1082644713497,208.));
#30865=CARTESIAN_POINT('Ctrl Pts',(84.6429883504424,74.9389576587352,208.093749998303));
#30866=CARTESIAN_POINT('Ctrl Pts',(85.4750748512497,78.3600352167018,208.187499995903));
#30867=CARTESIAN_POINT('Ctrl Pts',(86.3071613733569,81.781112862242,208.281249995903));
#30868=CARTESIAN_POINT('Ctrl Pts',(84.4764681935457,84.7885540866852,208.374999995903));
#30869=CARTESIAN_POINT('Ctrl Pts',(82.6457750137345,87.7959953111284,208.468749995903));
#30870=CARTESIAN_POINT('Ctrl Pts',(79.2246973681942,88.6280818332357,208.562499995903));
#30871=CARTESIAN_POINT('Ctrl Pts',(75.803619722654,89.460168355343,208.656249995903));
#30872=CARTESIAN_POINT('Ctrl Pts',(72.7961784982108,87.6294751755317,208.749999995903));
#30873=CARTESIAN_POINT('Ctrl Pts',(69.7887372737676,85.7987819957205,208.843749995903));
#30874=CARTESIAN_POINT('Ctrl Pts',(68.9566507516603,82.3777043501803,208.937499995903));
#30875=CARTESIAN_POINT('Ctrl Pts',(68.124564229553,78.95662670464,209.031249995903));
#30876=CARTESIAN_POINT('Ctrl Pts',(69.9552574093643,75.9491854801968,209.124999995903));
#30877=CARTESIAN_POINT('Ctrl Pts',(71.7859505891755,72.9417442557536,209.218749995903));
#30878=CARTESIAN_POINT('Ctrl Pts',(75.2070282347158,72.1096577336463,209.312499995903));
#30879=CARTESIAN_POINT('Ctrl Pts',(81.6355472361212,73.1082644713497,208.));
#30880=CARTESIAN_POINT('Ctrl Pts',(80.8763023374092,72.6460959996179,207.976332302027));
#30881=CARTESIAN_POINT('Ctrl Pts',(80.0492000646897,72.3058399894939,207.951271393806));
#30882=CARTESIAN_POINT('Ctrl Pts',(78.3088074180245,71.8915116109437,207.899872573309));
#30883=CARTESIAN_POINT('Ctrl Pts',(77.4056191879471,71.8234526459273,207.87384897067));
#30884=CARTESIAN_POINT('Ctrl Pts',(75.4144643689082,71.9896960664897,207.81787699499));
#30885=CARTESIAN_POINT('Ctrl Pts',(74.3483000261168,72.2921953447178,207.789415502797));
#30886=CARTESIAN_POINT('Ctrl Pts',(72.3787421826247,73.2917323325248,207.726588879605));
#30887=CARTESIAN_POINT('Ctrl Pts',(71.4963547690888,73.9836631758121,207.694289190011));
#30888=CARTESIAN_POINT('Ctrl Pts',(70.0567962100578,75.6571168902924,207.632330501293));
#30889=CARTESIAN_POINT('Ctrl Pts',(69.5092102801739,76.619155890067,207.603946128111));
#30890=CARTESIAN_POINT('Ctrl Pts',(68.8050736208812,78.712263806775,207.541219969294));
#30891=CARTESIAN_POINT('Ctrl Pts',(68.6607351367236,79.8252454036478,207.508884056451));
#30892=CARTESIAN_POINT('Ctrl Pts',(68.8075917415253,82.0275556159198,207.446812675813));
#30893=CARTESIAN_POINT('Ctrl Pts',(69.0911351356286,83.0963336594984,207.418492485847));
#30894=CARTESIAN_POINT('Ctrl Pts',(70.0557013989788,85.0826730046347,207.355870265652));
#30895=CARTESIAN_POINT('Ctrl Pts',(70.7335105098385,85.9784128363935,207.32350012221));
#30896=CARTESIAN_POINT('Ctrl Pts',(72.3821140895016,87.4457835655045,207.261317041861));
#30897=CARTESIAN_POINT('Ctrl Pts',(73.3325145913956,88.0087284623981,207.233047488343));
#30898=CARTESIAN_POINT('Ctrl Pts',(75.4124942858855,88.7496733152931,207.170532376289));
#30899=CARTESIAN_POINT('Ctrl Pts',(76.524761081961,88.9135985745502,207.138130168159));
#30900=CARTESIAN_POINT('Ctrl Pts',(78.1735146408528,88.8318190807521,207.091535997759));
#30901=CARTESIAN_POINT('Ctrl Pts',(78.7050820316669,88.7544645006295,207.07673935053));
#30902=CARTESIAN_POINT('Ctrl Pts',(79.2246973681942,88.6280818332357,207.062499995903));
#30903=CARTESIAN_POINT('Ctrl Pts',(75.3989071052151,72.8985570813421,196.468749997952));
#30904=CARTESIAN_POINT('Ctrl Pts',(78.4932119415925,72.1459493897285,196.562499997952));
#30905=CARTESIAN_POINT('Ctrl Pts',(81.2133898767664,73.8017793202762,196.656249997952));
#30906=CARTESIAN_POINT('Ctrl Pts',(83.9335678119403,75.4576092508238,196.749999997952));
#30907=CARTESIAN_POINT('Ctrl Pts',(84.6861755035539,78.5519140872012,196.843749997952));
#30908=CARTESIAN_POINT('Ctrl Pts',(85.4387831951675,81.6462189235785,196.937499997952));
#30909=CARTESIAN_POINT('Ctrl Pts',(83.7829532646199,84.3663968587524,197.031249997952));
#30910=CARTESIAN_POINT('Ctrl Pts',(82.1271233340723,87.0865747939263,197.124999997952));
#30911=CARTESIAN_POINT('Ctrl Pts',(79.0328184976949,87.83918248554,197.218749997952));
#30912=CARTESIAN_POINT('Ctrl Pts',(75.9385136613175,88.5917901771536,197.312499997952));
#30913=CARTESIAN_POINT('Ctrl Pts',(73.2183357261436,86.9359602466059,197.406249997952));
#30914=CARTESIAN_POINT('Ctrl Pts',(70.4981577909697,85.2801303160583,197.499999997952));
#30915=CARTESIAN_POINT('Ctrl Pts',(69.7455500993561,82.1858254796809,197.593749997952));
#30916=CARTESIAN_POINT('Ctrl Pts',(68.9929424077425,79.0915206433035,197.687499997952));
#30917=CARTESIAN_POINT('Ctrl Pts',(70.6487723382901,76.3713427081296,197.781249997952));
#30918=CARTESIAN_POINT('Ctrl Pts',(72.3046022688378,73.6511647729557,197.874999997952));
#30919=CARTESIAN_POINT('Ctrl Pts',(75.3989071052151,72.8985570813421,197.968749997952));
#30920=CARTESIAN_POINT('Ctrl Pts',(78.4932119415925,72.1459493897285,198.062499997952));
#30921=CARTESIAN_POINT('Ctrl Pts',(81.2133898767664,73.8017793202762,198.156249997952));
#30922=CARTESIAN_POINT('Ctrl Pts',(83.9335678119403,75.4576092508238,198.249999997952));
#30923=CARTESIAN_POINT('Ctrl Pts',(84.6861755035539,78.5519140872012,198.343749997952));
#30924=CARTESIAN_POINT('Ctrl Pts',(85.4387831951675,81.6462189235785,198.437499997952));
#30925=CARTESIAN_POINT('Ctrl Pts',(83.7829532646199,84.3663968587524,198.531249997952));
#30926=CARTESIAN_POINT('Ctrl Pts',(82.1271233340723,87.0865747939263,198.624999997952));
#30927=CARTESIAN_POINT('Ctrl Pts',(79.0328184976949,87.8391824855399,198.718749997952));
#30928=CARTESIAN_POINT('Ctrl Pts',(75.9385136613175,88.5917901771536,198.812499997952));
#30929=CARTESIAN_POINT('Ctrl Pts',(73.2183357261436,86.9359602466059,198.906249997952));
#30930=CARTESIAN_POINT('Ctrl Pts',(70.4981577909697,85.2801303160583,198.999999997952));
#30931=CARTESIAN_POINT('Ctrl Pts',(69.7455500993561,82.1858254796809,199.093749997952));
#30932=CARTESIAN_POINT('Ctrl Pts',(68.9929424077425,79.0915206433035,199.187499997952));
#30933=CARTESIAN_POINT('Ctrl Pts',(70.6487723382901,76.3713427081296,199.281249997952));
#30934=CARTESIAN_POINT('Ctrl Pts',(72.3046022688378,73.6511647729557,199.374999997952));
#30935=CARTESIAN_POINT('Ctrl Pts',(75.3989071052151,72.8985570813421,199.468749997952));
#30936=CARTESIAN_POINT('Ctrl Pts',(78.4932119415925,72.1459493897285,199.562499997952));
#30937=CARTESIAN_POINT('Ctrl Pts',(81.2133898767664,73.8017793202761,199.656249997952));
#30938=CARTESIAN_POINT('Ctrl Pts',(83.9335678119403,75.4576092508238,199.749999997952));
#30939=CARTESIAN_POINT('Ctrl Pts',(84.6861755035539,78.5519140872012,199.843749997952));
#30940=CARTESIAN_POINT('Ctrl Pts',(85.4387831951675,81.6462189235785,199.937499997952));
#30941=CARTESIAN_POINT('Ctrl Pts',(83.7829532646199,84.3663968587524,200.031249997952));
#30942=CARTESIAN_POINT('Ctrl Pts',(82.1271233340723,87.0865747939263,200.124999997952));
#30943=CARTESIAN_POINT('Ctrl Pts',(79.0328184976949,87.8391824855399,200.218749997952));
#30944=CARTESIAN_POINT('Ctrl Pts',(75.9385136613175,88.5917901771536,200.312499997952));
#30945=CARTESIAN_POINT('Ctrl Pts',(73.2183357261436,86.9359602466059,200.406249997952));
#30946=CARTESIAN_POINT('Ctrl Pts',(70.4981577909697,85.2801303160583,200.499999997952));
#30947=CARTESIAN_POINT('Ctrl Pts',(69.7455500993561,82.1858254796809,200.593749997952));
#30948=CARTESIAN_POINT('Ctrl Pts',(68.9929424077425,79.0915206433035,200.687499997952));
#30949=CARTESIAN_POINT('Ctrl Pts',(70.6487723382901,76.3713427081296,200.781249997952));
#30950=CARTESIAN_POINT('Ctrl Pts',(72.3046022688378,73.6511647729557,200.874999997952));
#30951=CARTESIAN_POINT('Ctrl Pts',(75.3989071052151,72.8985570813421,200.968749997952));
#30952=CARTESIAN_POINT('Ctrl Pts',(78.4932119415925,72.1459493897285,201.062499997952));
#30953=CARTESIAN_POINT('Ctrl Pts',(81.2133898767664,73.8017793202761,201.156249997952));
#30954=CARTESIAN_POINT('Ctrl Pts',(83.9335678119403,75.4576092508238,201.249999997952));
#30955=CARTESIAN_POINT('Ctrl Pts',(84.6861755035539,78.5519140872011,201.343749997952));
#30956=CARTESIAN_POINT('Ctrl Pts',(85.4387831951675,81.6462189235785,201.437499997952));
#30957=CARTESIAN_POINT('Ctrl Pts',(83.7829532646199,84.3663968587524,201.531249997952));
#30958=CARTESIAN_POINT('Ctrl Pts',(82.1271233340723,87.0865747939263,201.624999997952));
#30959=CARTESIAN_POINT('Ctrl Pts',(79.0328184976949,87.8391824855399,201.718749997952));
#30960=CARTESIAN_POINT('Ctrl Pts',(75.9385136613175,88.5917901771536,201.812499997952));
#30961=CARTESIAN_POINT('Ctrl Pts',(73.2183357261436,86.9359602466059,201.906249997952));
#30962=CARTESIAN_POINT('Ctrl Pts',(70.4981577909697,85.2801303160583,201.999999997952));
#30963=CARTESIAN_POINT('Ctrl Pts',(69.7455500993561,82.1858254796809,202.093749997952));
#30964=CARTESIAN_POINT('Ctrl Pts',(68.9929424077425,79.0915206433035,202.187499997952));
#30965=CARTESIAN_POINT('Ctrl Pts',(70.6487723382901,76.3713427081296,202.281249997952));
#30966=CARTESIAN_POINT('Ctrl Pts',(72.3046022688378,73.6511647729557,202.374999997952));
#30967=CARTESIAN_POINT('Ctrl Pts',(75.3989071052151,72.8985570813421,202.468749997952));
#30968=CARTESIAN_POINT('Ctrl Pts',(78.4932119415925,72.1459493897285,202.562499997952));
#30969=CARTESIAN_POINT('Ctrl Pts',(81.2133898767664,73.8017793202761,202.656249997952));
#30970=CARTESIAN_POINT('Ctrl Pts',(83.9335678119403,75.4576092508238,202.749999997952));
#30971=CARTESIAN_POINT('Ctrl Pts',(84.6861755035539,78.5519140872011,202.843749997952));
#30972=CARTESIAN_POINT('Ctrl Pts',(85.4387831951675,81.6462189235785,202.937499997952));
#30973=CARTESIAN_POINT('Ctrl Pts',(83.7829532646199,84.3663968587524,203.031249997952));
#30974=CARTESIAN_POINT('Ctrl Pts',(82.1271233340723,87.0865747939263,203.124999997952));
#30975=CARTESIAN_POINT('Ctrl Pts',(79.0328184976949,87.8391824855399,203.218749997952));
#30976=CARTESIAN_POINT('Ctrl Pts',(75.9385136613175,88.5917901771535,203.312499997952));
#30977=CARTESIAN_POINT('Ctrl Pts',(73.2183357261436,86.9359602466059,203.406249997952));
#30978=CARTESIAN_POINT('Ctrl Pts',(70.4981577909697,85.2801303160583,203.499999997952));
#30979=CARTESIAN_POINT('Ctrl Pts',(69.7455500993561,82.1858254796809,203.593749997952));
#30980=CARTESIAN_POINT('Ctrl Pts',(68.9929424077425,79.0915206433035,203.687499997952));
#30981=CARTESIAN_POINT('Ctrl Pts',(70.6487723382901,76.3713427081296,203.781249997952));
#30982=CARTESIAN_POINT('Ctrl Pts',(72.3046022688378,73.6511647729557,203.874999997952));
#30983=CARTESIAN_POINT('Ctrl Pts',(75.3989071052151,72.8985570813421,203.968749997952));
#30984=CARTESIAN_POINT('Ctrl Pts',(78.4932119415925,72.1459493897285,204.062499997952));
#30985=CARTESIAN_POINT('Ctrl Pts',(81.2133898767664,73.8017793202761,204.156249997952));
#30986=CARTESIAN_POINT('Ctrl Pts',(83.9335678119403,75.4576092508238,204.249999997952));
#30987=CARTESIAN_POINT('Ctrl Pts',(84.6861755035539,78.5519140872011,204.343749997952));
#30988=CARTESIAN_POINT('Ctrl Pts',(85.4387831951675,81.6462189235785,204.437499997952));
#30989=CARTESIAN_POINT('Ctrl Pts',(83.7829532646199,84.3663968587524,204.531249997952));
#30990=CARTESIAN_POINT('Ctrl Pts',(82.1271233340722,87.0865747939263,204.624999997952));
#30991=CARTESIAN_POINT('Ctrl Pts',(79.0328184976949,87.8391824855399,204.718749997952));
#30992=CARTESIAN_POINT('Ctrl Pts',(75.9385136613175,88.5917901771535,204.812499997952));
#30993=CARTESIAN_POINT('Ctrl Pts',(73.2183357261436,86.9359602466059,204.906249997952));
#30994=CARTESIAN_POINT('Ctrl Pts',(70.4981577909697,85.2801303160583,204.999999997952));
#30995=CARTESIAN_POINT('Ctrl Pts',(69.7455500993561,82.1858254796809,205.093749997952));
#30996=CARTESIAN_POINT('Ctrl Pts',(68.9929424077425,79.0915206433035,205.187499997952));
#30997=CARTESIAN_POINT('Ctrl Pts',(70.6487723382901,76.3713427081296,205.281249997952));
#30998=CARTESIAN_POINT('Ctrl Pts',(72.3046022688378,73.6511647729557,205.374999997952));
#30999=CARTESIAN_POINT('Ctrl Pts',(75.3989071052151,72.8985570813421,205.468749997952));
#31000=CARTESIAN_POINT('Ctrl Pts',(78.4932119415925,72.1459493897285,205.562499997952));
#31001=CARTESIAN_POINT('Ctrl Pts',(81.2133898767664,73.8017793202761,205.656249997952));
#31002=CARTESIAN_POINT('Ctrl Pts',(83.9335678119403,75.4576092508238,205.749999997952));
#31003=CARTESIAN_POINT('Ctrl Pts',(84.6861755035539,78.5519140872011,205.843749997952));
#31004=CARTESIAN_POINT('Ctrl Pts',(85.4387831951675,81.6462189235785,205.937499997952));
#31005=CARTESIAN_POINT('Ctrl Pts',(83.7829532646199,84.3663968587524,206.031249997952));
#31006=CARTESIAN_POINT('Ctrl Pts',(82.1271233340722,87.0865747939263,206.124999997952));
#31007=CARTESIAN_POINT('Ctrl Pts',(79.0328184976949,87.8391824855399,206.218749997952));
#31008=CARTESIAN_POINT('Ctrl Pts',(75.9385136613175,88.5917901771535,206.312499997952));
#31009=CARTESIAN_POINT('Ctrl Pts',(73.2183357261436,86.9359602466059,206.406249997952));
#31010=CARTESIAN_POINT('Ctrl Pts',(70.4981577909697,85.2801303160583,206.499999997952));
#31011=CARTESIAN_POINT('Ctrl Pts',(69.7455500993561,82.1858254796809,206.593749997952));
#31012=CARTESIAN_POINT('Ctrl Pts',(68.9929424077425,79.0915206433035,206.687499997952));
#31013=CARTESIAN_POINT('Ctrl Pts',(70.6487723382901,76.3713427081296,206.781249997952));
#31014=CARTESIAN_POINT('Ctrl Pts',(72.3046022688378,73.6511647729557,206.874999997952));
#31015=CARTESIAN_POINT('Ctrl Pts',(75.3989071052151,72.8985570813421,206.968749997952));
#31016=CARTESIAN_POINT('Ctrl Pts',(78.4932119415925,72.1459493897285,207.062499997952));
#31017=CARTESIAN_POINT('Ctrl Pts',(81.2133898767664,73.8017793202761,207.156249997952));
#31018=CARTESIAN_POINT('Ctrl Pts',(83.9335678119403,75.4576092508238,207.249999997952));
#31019=CARTESIAN_POINT('Ctrl Pts',(84.6861755035539,78.5519140872011,207.343749997952));
#31020=CARTESIAN_POINT('Ctrl Pts',(85.4387831951675,81.6462189235785,207.437499997952));
#31021=CARTESIAN_POINT('Ctrl Pts',(83.7829532646199,84.3663968587524,207.531249997952));
#31022=CARTESIAN_POINT('Ctrl Pts',(82.1271233340722,87.0865747939263,207.624999997952));
#31023=CARTESIAN_POINT('Ctrl Pts',(79.0328184976949,87.8391824855399,207.718749997952));
#31024=CARTESIAN_POINT('Ctrl Pts',(75.9385136613175,88.5917901771535,207.812499997952));
#31025=CARTESIAN_POINT('Ctrl Pts',(73.2183357261436,86.9359602466059,207.906249997952));
#31026=CARTESIAN_POINT('Ctrl Pts',(70.4981577909697,85.2801303160583,207.999999997952));
#31027=CARTESIAN_POINT('Ctrl Pts',(69.7455500993561,82.1858254796809,208.093749997952));
#31028=CARTESIAN_POINT('Ctrl Pts',(68.9929424077425,79.0915206433035,208.187499997952));
#31029=CARTESIAN_POINT('Ctrl Pts',(70.6487723382901,76.3713427081296,208.281249997952));
#31030=CARTESIAN_POINT('Ctrl Pts',(72.3046022688377,73.6511647729557,208.374999997952));
#31031=CARTESIAN_POINT('Ctrl Pts',(75.3989071052151,72.8985570813421,208.468749997952));
#31032=CARTESIAN_POINT('Ctrl Pts',(75.2070234291834,72.1096379759661,195.999988260337));
#31033=CARTESIAN_POINT('Ctrl Pts',(78.6281092586227,71.2775494633421,196.093738260337));
#31034=CARTESIAN_POINT('Ctrl Pts',(81.6355576774644,73.108247022536,196.187488260337));
#31035=CARTESIAN_POINT('Ctrl Pts',(84.643006096306,74.93894458173,196.281238260337));
#31036=CARTESIAN_POINT('Ctrl Pts',(85.47509460893,78.3600304111694,196.374988260337));
#31037=CARTESIAN_POINT('Ctrl Pts',(86.3071831215539,81.7811162406088,196.468738260337));
#31038=CARTESIAN_POINT('Ctrl Pts',(84.47648556236,84.7885646594504,196.562488260337));
#31039=CARTESIAN_POINT('Ctrl Pts',(82.645788003166,87.796013078292,196.656238260337));
#31040=CARTESIAN_POINT('Ctrl Pts',(79.2247021737267,88.628101590916,196.749988260337));
#31041=CARTESIAN_POINT('Ctrl Pts',(75.8036163442873,89.46019010354,196.843738260337));
#31042=CARTESIAN_POINT('Ctrl Pts',(72.7961679254456,87.629492544346,196.937488260337));
#31043=CARTESIAN_POINT('Ctrl Pts',(69.788719506604,85.7987949851521,197.031238260337));
#31044=CARTESIAN_POINT('Ctrl Pts',(68.95663099398,82.3777091557127,197.124988260337));
#31045=CARTESIAN_POINT('Ctrl Pts',(68.1245424813561,78.9566233262733,197.218738260337));
#31046=CARTESIAN_POINT('Ctrl Pts',(69.95524004055,75.9491749074317,197.312488260337));
#31047=CARTESIAN_POINT('Ctrl Pts',(71.785937599744,72.94172648859,197.406238260337));
#31048=CARTESIAN_POINT('Ctrl Pts',(75.2070234291834,72.1096379759661,197.499988260337));
#31049=CARTESIAN_POINT('Ctrl Pts',(78.6281092586227,71.2775494633421,197.593738260337));
#31050=CARTESIAN_POINT('Ctrl Pts',(81.6355576774644,73.108247022536,197.687488260337));
#31051=CARTESIAN_POINT('Ctrl Pts',(84.643006096306,74.93894458173,197.781238260337));
#31052=CARTESIAN_POINT('Ctrl Pts',(85.47509460893,78.3600304111694,197.874988260337));
#31053=CARTESIAN_POINT('Ctrl Pts',(86.3071831215539,81.7811162406088,197.968738260337));
#31054=CARTESIAN_POINT('Ctrl Pts',(84.47648556236,84.7885646594504,198.062488260337));
#31055=CARTESIAN_POINT('Ctrl Pts',(82.645788003166,87.796013078292,198.156238260337));
#31056=CARTESIAN_POINT('Ctrl Pts',(79.2247021737267,88.628101590916,198.249988260337));
#31057=CARTESIAN_POINT('Ctrl Pts',(75.8036163442873,89.46019010354,198.343738260337));
#31058=CARTESIAN_POINT('Ctrl Pts',(72.7961679254456,87.629492544346,198.437488260337));
#31059=CARTESIAN_POINT('Ctrl Pts',(69.788719506604,85.7987949851521,198.531238260337));
#31060=CARTESIAN_POINT('Ctrl Pts',(68.95663099398,82.3777091557127,198.624988260337));
#31061=CARTESIAN_POINT('Ctrl Pts',(68.1245424813561,78.9566233262733,198.718738260337));
#31062=CARTESIAN_POINT('Ctrl Pts',(69.95524004055,75.9491749074317,198.812488260337));
#31063=CARTESIAN_POINT('Ctrl Pts',(71.785937599744,72.94172648859,198.906238260337));
#31064=CARTESIAN_POINT('Ctrl Pts',(75.2070234291834,72.1096379759661,198.999988260337));
#31065=CARTESIAN_POINT('Ctrl Pts',(78.6281092586227,71.2775494633421,199.093738260337));
#31066=CARTESIAN_POINT('Ctrl Pts',(81.6355576774644,73.108247022536,199.187488260337));
#31067=CARTESIAN_POINT('Ctrl Pts',(84.643006096306,74.93894458173,199.281238260337));
#31068=CARTESIAN_POINT('Ctrl Pts',(85.47509460893,78.3600304111694,199.374988260337));
#31069=CARTESIAN_POINT('Ctrl Pts',(86.3071831215539,81.7811162406088,199.468738260337));
#31070=CARTESIAN_POINT('Ctrl Pts',(84.47648556236,84.7885646594504,199.562488260337));
#31071=CARTESIAN_POINT('Ctrl Pts',(82.645788003166,87.796013078292,199.656238260337));
#31072=CARTESIAN_POINT('Ctrl Pts',(79.2247021737267,88.628101590916,199.749988260337));
#31073=CARTESIAN_POINT('Ctrl Pts',(75.8036163442873,89.46019010354,199.843738260337));
#31074=CARTESIAN_POINT('Ctrl Pts',(72.7961679254456,87.629492544346,199.937488260337));
#31075=CARTESIAN_POINT('Ctrl Pts',(69.788719506604,85.7987949851521,200.031238260337));
#31076=CARTESIAN_POINT('Ctrl Pts',(68.95663099398,82.3777091557127,200.124988260337));
#31077=CARTESIAN_POINT('Ctrl Pts',(68.1245424813561,78.9566233262733,200.218738260337));
#31078=CARTESIAN_POINT('Ctrl Pts',(69.95524004055,75.9491749074317,200.312488260337));
#31079=CARTESIAN_POINT('Ctrl Pts',(71.785937599744,72.94172648859,200.406238260337));
#31080=CARTESIAN_POINT('Ctrl Pts',(75.2070234291834,72.1096379759661,200.499988260337));
#31081=CARTESIAN_POINT('Ctrl Pts',(78.6281092586227,71.2775494633421,200.593738260337));
#31082=CARTESIAN_POINT('Ctrl Pts',(81.6355576774644,73.108247022536,200.687488260337));
#31083=CARTESIAN_POINT('Ctrl Pts',(84.643006096306,74.93894458173,200.781238260337));
#31084=CARTESIAN_POINT('Ctrl Pts',(85.47509460893,78.3600304111694,200.874988260337));
#31085=CARTESIAN_POINT('Ctrl Pts',(86.3071831215539,81.7811162406088,200.968738260337));
#31086=CARTESIAN_POINT('Ctrl Pts',(84.47648556236,84.7885646594504,201.062488260337));
#31087=CARTESIAN_POINT('Ctrl Pts',(82.645788003166,87.796013078292,201.156238260337));
#31088=CARTESIAN_POINT('Ctrl Pts',(79.2247021737267,88.628101590916,201.249988260337));
#31089=CARTESIAN_POINT('Ctrl Pts',(75.8036163442873,89.46019010354,201.343738260337));
#31090=CARTESIAN_POINT('Ctrl Pts',(72.7961679254456,87.629492544346,201.437488260337));
#31091=CARTESIAN_POINT('Ctrl Pts',(69.788719506604,85.7987949851521,201.531238260337));
#31092=CARTESIAN_POINT('Ctrl Pts',(68.95663099398,82.3777091557127,201.624988260337));
#31093=CARTESIAN_POINT('Ctrl Pts',(68.1245424813561,78.9566233262733,201.718738260337));
#31094=CARTESIAN_POINT('Ctrl Pts',(69.95524004055,75.9491749074317,201.812488260337));
#31095=CARTESIAN_POINT('Ctrl Pts',(71.785937599744,72.94172648859,201.906238260337));
#31096=CARTESIAN_POINT('Ctrl Pts',(75.2070234291834,72.1096379759661,201.999988260337));
#31097=CARTESIAN_POINT('Ctrl Pts',(78.6281092586227,71.2775494633421,202.093738260337));
#31098=CARTESIAN_POINT('Ctrl Pts',(81.6355576774644,73.108247022536,202.187488260337));
#31099=CARTESIAN_POINT('Ctrl Pts',(84.643006096306,74.93894458173,202.281238260337));
#31100=CARTESIAN_POINT('Ctrl Pts',(85.47509460893,78.3600304111694,202.374988260337));
#31101=CARTESIAN_POINT('Ctrl Pts',(86.3071831215539,81.7811162406088,202.468738260337));
#31102=CARTESIAN_POINT('Ctrl Pts',(84.47648556236,84.7885646594504,202.562488260337));
#31103=CARTESIAN_POINT('Ctrl Pts',(82.645788003166,87.796013078292,202.656238260337));
#31104=CARTESIAN_POINT('Ctrl Pts',(79.2247021737267,88.628101590916,202.749988260337));
#31105=CARTESIAN_POINT('Ctrl Pts',(75.8036163442873,89.46019010354,202.843738260337));
#31106=CARTESIAN_POINT('Ctrl Pts',(72.7961679254456,87.629492544346,202.937488260337));
#31107=CARTESIAN_POINT('Ctrl Pts',(69.788719506604,85.7987949851521,203.031238260337));
#31108=CARTESIAN_POINT('Ctrl Pts',(68.95663099398,82.3777091557127,203.124988260337));
#31109=CARTESIAN_POINT('Ctrl Pts',(68.1245424813561,78.9566233262733,203.218738260337));
#31110=CARTESIAN_POINT('Ctrl Pts',(69.95524004055,75.9491749074317,203.312488260337));
#31111=CARTESIAN_POINT('Ctrl Pts',(71.785937599744,72.94172648859,203.406238260337));
#31112=CARTESIAN_POINT('Ctrl Pts',(75.2070234291834,72.1096379759661,203.499988260337));
#31113=CARTESIAN_POINT('Ctrl Pts',(78.6281092586227,71.2775494633421,203.593738260337));
#31114=CARTESIAN_POINT('Ctrl Pts',(81.6355576774644,73.108247022536,203.687488260337));
#31115=CARTESIAN_POINT('Ctrl Pts',(84.643006096306,74.93894458173,203.781238260337));
#31116=CARTESIAN_POINT('Ctrl Pts',(85.47509460893,78.3600304111694,203.874988260337));
#31117=CARTESIAN_POINT('Ctrl Pts',(86.3071831215539,81.7811162406088,203.968738260337));
#31118=CARTESIAN_POINT('Ctrl Pts',(84.47648556236,84.7885646594504,204.062488260337));
#31119=CARTESIAN_POINT('Ctrl Pts',(82.645788003166,87.796013078292,204.156238260337));
#31120=CARTESIAN_POINT('Ctrl Pts',(79.2247021737267,88.628101590916,204.249988260337));
#31121=CARTESIAN_POINT('Ctrl Pts',(75.8036163442873,89.46019010354,204.343738260337));
#31122=CARTESIAN_POINT('Ctrl Pts',(72.7961679254456,87.629492544346,204.437488260337));
#31123=CARTESIAN_POINT('Ctrl Pts',(69.788719506604,85.7987949851521,204.531238260337));
#31124=CARTESIAN_POINT('Ctrl Pts',(68.95663099398,82.3777091557127,204.624988260337));
#31125=CARTESIAN_POINT('Ctrl Pts',(68.1245424813561,78.9566233262733,204.718738260337));
#31126=CARTESIAN_POINT('Ctrl Pts',(69.95524004055,75.9491749074317,204.812488260337));
#31127=CARTESIAN_POINT('Ctrl Pts',(71.785937599744,72.94172648859,204.906238260337));
#31128=CARTESIAN_POINT('Ctrl Pts',(75.2070234291834,72.1096379759661,204.999988260337));
#31129=CARTESIAN_POINT('Ctrl Pts',(78.6281092586227,71.2775494633421,205.093738260337));
#31130=CARTESIAN_POINT('Ctrl Pts',(81.6355576774644,73.108247022536,205.187488260337));
#31131=CARTESIAN_POINT('Ctrl Pts',(84.643006096306,74.93894458173,205.281238260337));
#31132=CARTESIAN_POINT('Ctrl Pts',(85.47509460893,78.3600304111694,205.374988260337));
#31133=CARTESIAN_POINT('Ctrl Pts',(86.3071831215539,81.7811162406088,205.468738260337));
#31134=CARTESIAN_POINT('Ctrl Pts',(84.47648556236,84.7885646594504,205.562488260337));
#31135=CARTESIAN_POINT('Ctrl Pts',(82.645788003166,87.796013078292,205.656238260337));
#31136=CARTESIAN_POINT('Ctrl Pts',(79.2247021737267,88.628101590916,205.749988260337));
#31137=CARTESIAN_POINT('Ctrl Pts',(75.8036163442873,89.4601901035399,205.843738260337));
#31138=CARTESIAN_POINT('Ctrl Pts',(72.7961679254456,87.629492544346,205.937488260337));
#31139=CARTESIAN_POINT('Ctrl Pts',(69.788719506604,85.7987949851521,206.031238260337));
#31140=CARTESIAN_POINT('Ctrl Pts',(68.95663099398,82.3777091557127,206.124988260337));
#31141=CARTESIAN_POINT('Ctrl Pts',(68.1245424813561,78.9566233262733,206.218738260337));
#31142=CARTESIAN_POINT('Ctrl Pts',(69.95524004055,75.9491749074317,206.312488260337));
#31143=CARTESIAN_POINT('Ctrl Pts',(71.785937599744,72.94172648859,206.406238260337));
#31144=CARTESIAN_POINT('Ctrl Pts',(75.2070234291834,72.109637975966,206.499988260337));
#31145=CARTESIAN_POINT('Ctrl Pts',(78.6281092586227,71.2775494633421,206.593738260337));
#31146=CARTESIAN_POINT('Ctrl Pts',(81.6355576774644,73.108247022536,206.687488260337));
#31147=CARTESIAN_POINT('Ctrl Pts',(84.643006096306,74.93894458173,206.781238260337));
#31148=CARTESIAN_POINT('Ctrl Pts',(85.47509460893,78.3600304111694,206.874988260337));
#31149=CARTESIAN_POINT('Ctrl Pts',(86.3071831215539,81.7811162406088,206.968738260337));
#31150=CARTESIAN_POINT('Ctrl Pts',(84.47648556236,84.7885646594504,207.062488260337));
#31151=CARTESIAN_POINT('Ctrl Pts',(82.645788003166,87.796013078292,207.156238260337));
#31152=CARTESIAN_POINT('Ctrl Pts',(79.2247021737266,88.628101590916,207.249988260337));
#31153=CARTESIAN_POINT('Ctrl Pts',(75.8036163442873,89.4601901035399,207.343738260337));
#31154=CARTESIAN_POINT('Ctrl Pts',(72.7961679254456,87.629492544346,207.437488260337));
#31155=CARTESIAN_POINT('Ctrl Pts',(69.788719506604,85.7987949851521,207.531238260337));
#31156=CARTESIAN_POINT('Ctrl Pts',(68.95663099398,82.3777091557127,207.624988260337));
#31157=CARTESIAN_POINT('Ctrl Pts',(68.1245424813561,78.9566233262733,207.718738260337));
#31158=CARTESIAN_POINT('Ctrl Pts',(69.95524004055,75.9491749074317,207.812488260337));
#31159=CARTESIAN_POINT('Ctrl Pts',(71.785937599744,72.94172648859,207.906238260337));
#31160=CARTESIAN_POINT('Ctrl Pts',(75.2070234291834,72.109637975966,207.999988260337));
#31161=CARTESIAN_POINT('',(75.2070282347158,72.1096577336463,208.));
#31162=CARTESIAN_POINT('Ctrl Pts',(79.2246973785512,88.6280818307166,207.249999999716));
#31163=CARTESIAN_POINT('Ctrl Pts',(79.2165277293079,88.6300688815138,207.25022387789));
#31164=CARTESIAN_POINT('Ctrl Pts',(79.2083545666696,88.6320439481805,207.250447909143));
#31165=CARTESIAN_POINT('Ctrl Pts',(78.0953063455651,88.8992673886528,207.280964955017));
#31166=CARTESIAN_POINT('Ctrl Pts',(76.9484141012642,88.9403006829013,207.313446540827));
#31167=CARTESIAN_POINT('Ctrl Pts',(74.7496089525614,88.5762581883052,207.377678333948));
#31168=CARTESIAN_POINT('Ctrl Pts',(73.7162576426031,88.1916641629506,207.408769405604));
#31169=CARTESIAN_POINT('Ctrl Pts',(71.814354597471,87.0295873468618,207.468157984612));
#31170=CARTESIAN_POINT('Ctrl Pts',(70.9732538750771,86.2485920856208,207.500636005768));
#31171=CARTESIAN_POINT('Ctrl Pts',(69.673455491204,84.4377773413139,207.564876660879));
#31172=CARTESIAN_POINT('Ctrl Pts',(69.2134313752649,83.4355810486969,207.596008021778));
#31173=CARTESIAN_POINT('Ctrl Pts',(68.6876255490353,81.2693907373049,207.655374234711));
#31174=CARTESIAN_POINT('Ctrl Pts',(68.6437671802273,80.1223021883416,207.687848912984));
#31175=CARTESIAN_POINT('Ctrl Pts',(69.0025977101215,77.9221893998447,207.752094889348));
#31176=CARTESIAN_POINT('Ctrl Pts',(69.3848062472608,76.8876831559372,207.783248195099));
#31177=CARTESIAN_POINT('Ctrl Pts',(70.542588686374,74.9829099000098,207.842617588817));
#31178=CARTESIAN_POINT('Ctrl Pts',(71.3215831173499,74.1399909718324,207.875063759399));
#31179=CARTESIAN_POINT('Ctrl Pts',(73.1336685807777,72.8328855994505,207.939458270806));
#31180=CARTESIAN_POINT('Ctrl Pts',(74.140174969224,72.3691415323959,207.970764331008));
#31181=CARTESIAN_POINT('Ctrl Pts',(75.2070282347158,72.1096577336464,208.));
#31182=CARTESIAN_POINT('',(75.3029676699654,72.5041074074942,208.234374998976));
#31183=CARTESIAN_POINT('',(75.3989071052151,72.8985570813421,196.468749997952));
#31184=CARTESIAN_POINT('Ctrl Pts',(75.3989071052151,72.8985570813421,196.468749997952));
#31185=CARTESIAN_POINT('Ctrl Pts',(78.4932119415925,72.1459493897285,196.562499997952));
#31186=CARTESIAN_POINT('Ctrl Pts',(81.2133898767664,73.8017793202762,196.656249997952));
#31187=CARTESIAN_POINT('Ctrl Pts',(83.9335678119403,75.4576092508238,196.749999997952));
#31188=CARTESIAN_POINT('Ctrl Pts',(84.6861755035539,78.5519140872012,196.843749997952));
#31189=CARTESIAN_POINT('Ctrl Pts',(85.4387831951675,81.6462189235786,196.937499997952));
#31190=CARTESIAN_POINT('Ctrl Pts',(83.7829532646199,84.3663968587524,197.031249997952));
#31191=CARTESIAN_POINT('Ctrl Pts',(82.1271233340723,87.0865747939263,197.124999997952));
#31192=CARTESIAN_POINT('Ctrl Pts',(79.0328184976949,87.83918248554,197.218749997952));
#31193=CARTESIAN_POINT('',(75.3029676699654,72.5041074074942,196.234374998976));
#31194=CARTESIAN_POINT('Origin',(75.3029676699654,72.5041074074942,196.234374998976));
#31195=CARTESIAN_POINT('',(75.3989071052151,72.8985570813421,196.656249997952));
#31196=CARTESIAN_POINT('Origin',(77.215862801455,80.3688697834411,196.));
#31197=CARTESIAN_POINT('',(75.7269618872836,74.2473361465344,196.));
#31198=CARTESIAN_POINT('Origin',(77.215862801455,80.3688697834411,196.));
#31199=CARTESIAN_POINT('Origin',(77.215862801455,80.368869783441,212.));
#31200=CARTESIAN_POINT('',(75.7978619308155,74.5388377482919,200.));
#31201=CARTESIAN_POINT('Origin',(77.215862801455,80.3688697834411,200.));
#31202=CARTESIAN_POINT('',(75.7978619308155,74.5388377482919,196.3));
#31203=CARTESIAN_POINT('',(75.7978619308155,74.5388377482918,212.));
#31204=CARTESIAN_POINT('Origin',(77.215862801455,80.3688697834411,196.3));
#31205=CARTESIAN_POINT('Origin',(77.215862801455,80.3688697834411,196.));
#31206=CARTESIAN_POINT('',(75.2070282347158,72.1096577336463,208.656249997952));
#31207=CARTESIAN_POINT('Origin',(77.215862801455,80.368869783441,208.));
#31208=CARTESIAN_POINT('Origin',(77.215862801455,80.368869783441,196.656249997952));
#31209=CARTESIAN_POINT('Origin',(75.3029676699654,72.5041074074942,208.234374998976));
#31210=CARTESIAN_POINT('Origin',(77.215862801455,80.3688697834411,196.3));
#31211=CARTESIAN_POINT('Origin',(75.7269618872836,74.2473361465344,196.3));
#31212=CARTESIAN_POINT('Origin',(77.215862801455,80.368869783441,208.3));
#31213=CARTESIAN_POINT('',(74.9234280605879,70.9436513266165,208.));
#31214=CARTESIAN_POINT('Origin',(77.215862801455,80.368869783441,208.));
#31215=CARTESIAN_POINT('',(74.8525280170559,70.652149724859,208.3));
#31216=CARTESIAN_POINT('Origin',(74.9234280605879,70.9436513266165,208.3));
#31217=CARTESIAN_POINT('',(79.5791975858541,90.085589842023,208.3));
#31218=CARTESIAN_POINT('Origin',(77.215862801455,80.368869783441,208.3));
#31219=CARTESIAN_POINT('Origin',(77.215862801455,80.368869783441,208.3));
#31220=CARTESIAN_POINT('Origin',(77.215862801455,80.368869783441,212.5));
#31221=CARTESIAN_POINT('',(76.0932787788654,75.7534277556146,212.5));
#31222=CARTESIAN_POINT('Origin',(77.215862801455,80.368869783441,212.5));
#31223=CARTESIAN_POINT('',(76.0932787788654,75.7534277556146,212.));
#31224=CARTESIAN_POINT('',(76.0932787788654,75.7534277556146,212.5));
#31225=CARTESIAN_POINT('Origin',(77.215862801455,80.368869783441,212.));
#31226=CARTESIAN_POINT('Origin',(77.215862801455,80.368869783441,212.5));
#31227=CARTESIAN_POINT('',(75.5615284523756,73.5671657424336,212.));
#31228=CARTESIAN_POINT('Origin',(77.215862801455,80.368869783441,212.));
#31229=CARTESIAN_POINT('',(75.5615284523756,73.5671657424336,212.5));
#31230=CARTESIAN_POINT('',(75.5615284523756,73.5671657424336,212.5));
#31231=CARTESIAN_POINT('Origin',(77.215862801455,80.368869783441,212.5));
#31232=CARTESIAN_POINT('Origin',(77.215862801455,80.368869783441,212.5));
#31233=CARTESIAN_POINT('Origin',(77.215862801455,80.368869783441,212.));
#31234=CARTESIAN_POINT('',(75.7978619308155,74.5388377482918,212.));
#31235=CARTESIAN_POINT('Origin',(77.215862801455,80.368869783441,212.));
#31236=CARTESIAN_POINT('Origin',(77.215862801455,80.368869783441,208.));
#31237=CARTESIAN_POINT('',(75.5529660276326,70.5081003246406,210.));
#31238=CARTESIAN_POINT('',(74.1641752411726,70.8458868981042,210.));
#31239=CARTESIAN_POINT('Origin',(77.215862801455,80.368869783441,210.));
#31240=CARTESIAN_POINT('',(67.3550933426544,82.0317665572624,210.));
#31241=CARTESIAN_POINT('Origin',(77.215862801455,80.368869783441,210.));
#31242=CARTESIAN_POINT('',(67.6928799161183,83.4205573437238,210.));
#31243=CARTESIAN_POINT('Origin',(77.215862801455,80.368869783441,210.));
#31244=CARTESIAN_POINT('',(78.8787595752761,90.2296392422416,210.));
#31245=CARTESIAN_POINT('Origin',(77.215862801455,80.368869783441,210.));
#31246=CARTESIAN_POINT('',(79.5791975858541,90.085589842023,210.));
#31247=CARTESIAN_POINT('Origin',(77.215862801455,80.368869783441,210.));
#31248=CARTESIAN_POINT('',(79.5791975858541,90.085589842023,208.));
#31249=CARTESIAN_POINT('',(80.2675503617385,89.8918526687775,210.));
#31250=CARTESIAN_POINT('Origin',(77.215862801455,80.368869783441,210.));
#31251=CARTESIAN_POINT('',(87.0766322602554,78.7059730096184,210.));
#31252=CARTESIAN_POINT('Origin',(77.215862801455,80.368869783441,210.));
#31253=CARTESIAN_POINT('',(86.7388456867917,77.3171822231584,210.));
#31254=CARTESIAN_POINT('Origin',(77.215862801455,80.368869783441,210.));
#31255=CARTESIAN_POINT('Origin',(77.215862801455,80.368869783441,210.));
#31256=CARTESIAN_POINT('Origin',(77.215862801455,80.368869783441,208.));
#31257=CARTESIAN_POINT('Origin',(77.215862801455,80.368869783441,208.));
#31258=CARTESIAN_POINT('Origin',(77.215862801455,80.368869783441,210.));
#31259=CARTESIAN_POINT('',(79.5201142162436,89.8426718405577,210.));
#31260=CARTESIAN_POINT('Origin',(79.8155310642937,91.057261847881,210.));
#31261=CARTESIAN_POINT('Origin',(79.8155310642937,91.057261847881,210.));
#31262=CARTESIAN_POINT('Origin',(77.215862801455,80.368869783441,210.));
#31263=CARTESIAN_POINT('Origin',(66.5274707370145,82.9685380462795,210.));
#31264=CARTESIAN_POINT('Origin',(77.215862801455,80.368869783441,210.));
#31265=CARTESIAN_POINT('Origin',(74.6161945386162,69.6804777190005,210.));
#31266=CARTESIAN_POINT('Origin',(77.215862801455,80.368869783441,210.));
#31267=CARTESIAN_POINT('Origin',(87.9042548658952,77.769201520602,210.));
#31268=CARTESIAN_POINT('Origin',(79.8155310642937,91.057261847881,212.));
#31269=CARTESIAN_POINT('',(79.5201142162436,89.8426718405577,212.));
#31270=CARTESIAN_POINT('Origin',(79.8155310642937,91.057261847881,212.));
#31271=CARTESIAN_POINT('',(79.5201142162436,89.8426718405577,212.));
#31272=CARTESIAN_POINT('Origin',(79.8155310642937,91.057261847881,210.));
#31273=CARTESIAN_POINT('Origin',(66.5274707370145,82.9685380462795,212.));
#31274=CARTESIAN_POINT('',(66.2320538889645,81.7539480389562,212.));
#31275=CARTESIAN_POINT('Origin',(66.5274707370145,82.9685380462795,212.));
#31276=CARTESIAN_POINT('',(66.2320538889645,81.7539480389562,210.));
#31277=CARTESIAN_POINT('',(66.2320538889645,81.7539480389562,212.));
#31278=CARTESIAN_POINT('Origin',(66.5274707370145,82.9685380462795,210.));
#31279=CARTESIAN_POINT('Origin',(66.5274707370145,82.9685380462795,210.));
#31280=CARTESIAN_POINT('Origin',(74.6161945386162,69.6804777190005,212.));
#31281=CARTESIAN_POINT('',(74.3207776905663,68.4658877116775,212.));
#31282=CARTESIAN_POINT('Origin',(74.6161945386162,69.6804777190005,212.));
#31283=CARTESIAN_POINT('',(74.3207776905663,68.4658877116775,210.));
#31284=CARTESIAN_POINT('',(74.3207776905663,68.4658877116775,212.));
#31285=CARTESIAN_POINT('Origin',(74.6161945386162,69.6804777190005,210.));
#31286=CARTESIAN_POINT('Origin',(74.6161945386162,69.6804777190005,210.));
#31287=CARTESIAN_POINT('Origin',(87.9042548658952,77.769201520602,212.));
#31288=CARTESIAN_POINT('',(87.6088380178453,76.5546115132792,212.));
#31289=CARTESIAN_POINT('Origin',(87.9042548658952,77.769201520602,212.));
#31290=CARTESIAN_POINT('',(87.6088380178453,76.5546115132792,210.));
#31291=CARTESIAN_POINT('',(87.6088380178453,76.5546115132792,212.));
#31292=CARTESIAN_POINT('Origin',(87.9042548658952,77.769201520602,210.));
#31293=CARTESIAN_POINT('Origin',(87.9042548658952,77.769201520602,210.));
#31294=CARTESIAN_POINT('Origin',(77.215862801455,80.368869783441,212.));
#31295=CARTESIAN_POINT('',(75.7978619308155,74.5388377482918,210.));
#31296=CARTESIAN_POINT('',(75.7978619308155,74.5388377482918,212.));
#31297=CARTESIAN_POINT('Origin',(77.215862801455,80.368869783441,210.));
#31298=CARTESIAN_POINT('Origin',(92.5196968937216,76.6466174980124,212.));
#31299=CARTESIAN_POINT('',(90.8192708834698,77.0602010852822,210.));
#31300=CARTESIAN_POINT('',(92.5196968937216,76.6466174980124,210.));
#31301=CARTESIAN_POINT('',(92.5196968937216,76.6466174980124,210.));
#31302=CARTESIAN_POINT('',(92.5196968937216,76.6466174980124,212.));
#31303=CARTESIAN_POINT('',(92.5196968937216,76.6466174980124,212.));
#31304=CARTESIAN_POINT('',(90.8192708834698,77.0602010852822,212.));
#31305=CARTESIAN_POINT('',(92.5196968937216,76.6466174980124,212.));
#31306=CARTESIAN_POINT('',(90.8192708834698,77.0602010852822,212.));
#31307=CARTESIAN_POINT('Origin',(91.8627047718599,74.593730778034,212.));
#31308=CARTESIAN_POINT('',(91.8627047718599,74.593730778034,210.));
#31309=CARTESIAN_POINT('',(91.8627047718599,74.593730778034,210.));
#31310=CARTESIAN_POINT('',(91.8627047718599,74.593730778034,212.));
#31311=CARTESIAN_POINT('',(91.8627047718599,74.593730778034,212.));
#31312=CARTESIAN_POINT('',(91.8627047718599,74.593730778034,212.));
#31313=CARTESIAN_POINT('Origin',(90.2363869009964,75.2399429590628,212.));
#31314=CARTESIAN_POINT('',(90.2363869009964,75.2399429590628,210.));
#31315=CARTESIAN_POINT('',(90.2363869009964,75.2399429590628,210.));
#31316=CARTESIAN_POINT('',(90.2363869009964,75.2399429590628,212.));
#31317=CARTESIAN_POINT('',(90.2363869009964,75.2399429590628,212.));
#31318=CARTESIAN_POINT('',(90.2363869009964,75.2399429590628,212.));
#31319=CARTESIAN_POINT('Origin',(90.9263998414264,72.6522582414015,212.));
#31320=CARTESIAN_POINT('',(90.9263998414264,72.6522582414015,210.));
#31321=CARTESIAN_POINT('',(90.9263998414264,72.6522582414015,210.));
#31322=CARTESIAN_POINT('',(90.9263998414264,72.6522582414015,212.));
#31323=CARTESIAN_POINT('',(90.9263998414264,72.6522582414015,212.));
#31324=CARTESIAN_POINT('',(90.9263998414264,72.6522582414015,212.));
#31325=CARTESIAN_POINT('Origin',(89.4058445373984,73.5185212311411,212.));
#31326=CARTESIAN_POINT('',(89.4058445373984,73.5185212311411,210.));
#31327=CARTESIAN_POINT('',(89.4058445373984,73.5185212311411,210.));
#31328=CARTESIAN_POINT('',(89.4058445373984,73.5185212311411,212.));
#31329=CARTESIAN_POINT('',(89.4058445373984,73.5185212311411,212.));
#31330=CARTESIAN_POINT('',(89.4058445373984,73.5185212311411,212.));
#31331=CARTESIAN_POINT('Origin',(89.7290062128608,70.8599884426483,212.));
#31332=CARTESIAN_POINT('',(89.7290062128608,70.8599884426483,210.));
#31333=CARTESIAN_POINT('',(89.7290062128608,70.8599884426483,210.));
#31334=CARTESIAN_POINT('',(89.7290062128608,70.8599884426483,212.));
#31335=CARTESIAN_POINT('',(89.7290062128608,70.8599884426483,212.));
#31336=CARTESIAN_POINT('',(89.7290062128608,70.8599884426483,212.));
#31337=CARTESIAN_POINT('Origin',(88.3438093550553,71.9294414173629,212.));
#31338=CARTESIAN_POINT('',(88.3438093550553,71.9294414173629,210.));
#31339=CARTESIAN_POINT('',(88.3438093550553,71.9294414173629,210.));
#31340=CARTESIAN_POINT('',(88.3438093550553,71.9294414173629,212.));
#31341=CARTESIAN_POINT('',(88.3438093550553,71.9294414173629,212.));
#31342=CARTESIAN_POINT('',(88.3438093550553,71.9294414173629,212.));
#31343=CARTESIAN_POINT('Origin',(88.2938297911282,69.2518058747305,212.));
#31344=CARTESIAN_POINT('',(88.2938297911282,69.2518058747305,210.));
#31345=CARTESIAN_POINT('',(88.2938297911282,69.2518058747305,210.));
#31346=CARTESIAN_POINT('',(88.2938297911282,69.2518058747305,212.));
#31347=CARTESIAN_POINT('',(88.2938297911282,69.2518058747305,212.));
#31348=CARTESIAN_POINT('',(88.2938297911282,69.2518058747305,212.));
#31349=CARTESIAN_POINT('Origin',(87.0709526607442,70.5036331487519,212.));
#31350=CARTESIAN_POINT('',(87.0709526607442,70.5036331487519,210.));
#31351=CARTESIAN_POINT('',(87.0709526607442,70.5036331487519,210.));
#31352=CARTESIAN_POINT('',(87.0709526607442,70.5036331487519,212.));
#31353=CARTESIAN_POINT('',(87.0709526607442,70.5036331487519,212.));
#31354=CARTESIAN_POINT('',(87.0709526607442,70.5036331487519,212.));
#31355=CARTESIAN_POINT('Origin',(86.6488046527885,67.8590119820519,212.));
#31356=CARTESIAN_POINT('',(86.6488046527885,67.8590119820519,210.));
#31357=CARTESIAN_POINT('',(86.6488046527885,67.8590119820519,210.));
#31358=CARTESIAN_POINT('',(86.6488046527885,67.8590119820519,212.));
#31359=CARTESIAN_POINT('',(86.6488046527885,67.8590119820519,212.));
#31360=CARTESIAN_POINT('',(86.6488046527885,67.8590119820519,212.));
#31361=CARTESIAN_POINT('Origin',(85.6120491621669,69.2688481614238,212.));
#31362=CARTESIAN_POINT('',(85.6120491621669,69.2688481614238,210.));
#31363=CARTESIAN_POINT('',(85.6120491621669,69.2688481614238,210.));
#31364=CARTESIAN_POINT('',(85.6120491621669,69.2688481614238,212.));
#31365=CARTESIAN_POINT('',(85.6120491621669,69.2688481614238,212.));
#31366=CARTESIAN_POINT('',(85.6120491621669,69.2688481614238,212.));
#31367=CARTESIAN_POINT('Origin',(84.8259493409712,66.708715913454,212.));
#31368=CARTESIAN_POINT('',(84.8259493409713,66.708715913454,210.));
#31369=CARTESIAN_POINT('',(84.8259493409713,66.708715913454,210.));
#31370=CARTESIAN_POINT('',(84.8259493409712,66.708715913454,212.));
#31371=CARTESIAN_POINT('',(84.8259493409712,66.708715913454,212.));
#31372=CARTESIAN_POINT('',(84.8259493409712,66.708715913454,212.));
#31373=CARTESIAN_POINT('Origin',(83.995494756445,68.2491201406098,212.));
#31374=CARTESIAN_POINT('',(83.995494756445,68.2491201406098,210.));
#31375=CARTESIAN_POINT('',(83.995494756445,68.2491201406098,210.));
#31376=CARTESIAN_POINT('',(83.995494756445,68.2491201406098,212.));
#31377=CARTESIAN_POINT('',(83.995494756445,68.2491201406098,212.));
#31378=CARTESIAN_POINT('',(83.995494756445,68.2491201406098,212.));
#31379=CARTESIAN_POINT('Origin',(82.8607436608537,65.8233068734697,212.));
#31380=CARTESIAN_POINT('',(82.8607436608537,65.8233068734697,210.));
#31381=CARTESIAN_POINT('',(82.8607436608537,65.8233068734697,210.));
#31382=CARTESIAN_POINT('',(82.8607436608537,65.8233068734697,212.));
#31383=CARTESIAN_POINT('',(82.8607436608537,65.8233068734697,212.));
#31384=CARTESIAN_POINT('',(82.8607436608537,65.8233068734697,212.));
#31385=CARTESIAN_POINT('Origin',(82.2527538362826,67.4642969323117,212.));
#31386=CARTESIAN_POINT('',(82.2527538362826,67.4642969323117,210.));
#31387=CARTESIAN_POINT('',(82.2527538362826,67.4642969323117,210.));
#31388=CARTESIAN_POINT('',(82.2527538362826,67.4642969323117,212.));
#31389=CARTESIAN_POINT('',(82.2527538362826,67.4642969323117,212.));
#31390=CARTESIAN_POINT('',(82.2527538362826,67.4642969323117,212.));
#31391=CARTESIAN_POINT('Origin',(80.791438105611,65.2200183419245,212.));
#31392=CARTESIAN_POINT('',(80.7914381056111,65.2200183419245,210.));
#31393=CARTESIAN_POINT('',(80.7914381056111,65.2200183419245,210.));
#31394=CARTESIAN_POINT('',(80.791438105611,65.2200183419245,212.));
#31395=CARTESIAN_POINT('',(80.791438105611,65.2200183419245,212.));
#31396=CARTESIAN_POINT('',(80.791438105611,65.2200183419245,212.));
#31397=CARTESIAN_POINT('Origin',(80.4177468713522,66.9296542275557,212.));
#31398=CARTESIAN_POINT('',(80.4177468713522,66.9296542275557,210.));
#31399=CARTESIAN_POINT('',(80.4177468713522,66.9296542275557,210.));
#31400=CARTESIAN_POINT('',(80.4177468713522,66.9296542275557,212.));
#31401=CARTESIAN_POINT('',(80.4177468713522,66.9296542275557,212.));
#31402=CARTESIAN_POINT('',(80.4177468713522,66.9296542275557,212.));
#31403=CARTESIAN_POINT('Origin',(78.6583093540759,64.9105926438542,212.));
#31404=CARTESIAN_POINT('',(78.6583093540759,64.9105926438542,210.));
#31405=CARTESIAN_POINT('',(78.6583093540759,64.9105926438542,210.));
#31406=CARTESIAN_POINT('',(78.6583093540759,64.9105926438542,212.));
#31407=CARTESIAN_POINT('',(78.6583093540759,64.9105926438542,212.));
#31408=CARTESIAN_POINT('',(78.6583093540759,64.9105926438542,212.));
#31409=CARTESIAN_POINT('Origin',(78.5261901849366,66.6555982384429,212.));
#31410=CARTESIAN_POINT('',(78.5261901849366,66.6555982384429,210.));
#31411=CARTESIAN_POINT('',(78.5261901849366,66.6555982384429,210.));
#31412=CARTESIAN_POINT('',(78.5261901849366,66.6555982384429,212.));
#31413=CARTESIAN_POINT('',(78.5261901849366,66.6555982384429,212.));
#31414=CARTESIAN_POINT('',(78.5261901849366,66.6555982384429,212.));
#31415=CARTESIAN_POINT('Origin',(76.5028763309989,64.9010523985053,212.));
#31416=CARTESIAN_POINT('',(76.5028763309989,64.9010523985053,210.));
#31417=CARTESIAN_POINT('',(76.5028763309989,64.9010523985053,210.));
#31418=CARTESIAN_POINT('',(76.5028763309989,64.9010523985053,212.));
#31419=CARTESIAN_POINT('',(76.5028763309989,64.9010523985053,212.));
#31420=CARTESIAN_POINT('',(76.5028763309989,64.9010523985053,212.));
#31421=CARTESIAN_POINT('Origin',(76.6149007763232,66.6474631530673,212.));
#31422=CARTESIAN_POINT('',(76.6149007763232,66.6474631530673,210.));
#31423=CARTESIAN_POINT('',(76.6149007763232,66.6474631530673,210.));
#31424=CARTESIAN_POINT('',(76.6149007763232,66.6474631530673,212.));
#31425=CARTESIAN_POINT('',(76.6149007763232,66.6474631530673,212.));
#31426=CARTESIAN_POINT('',(76.6149007763232,66.6474631530673,212.));
#31427=CARTESIAN_POINT('Origin',(74.3670920884055,65.1915832959018,212.));
#31428=CARTESIAN_POINT('',(74.3670920884055,65.1915832959018,210.));
#31429=CARTESIAN_POINT('',(74.3670920884055,65.1915832959018,210.));
#31430=CARTESIAN_POINT('',(74.3670920884055,65.1915832959018,212.));
#31431=CARTESIAN_POINT('',(74.3670920884055,65.1915832959018,212.));
#31432=CARTESIAN_POINT('',(74.3670920884055,65.1915832959018,212.));
#31433=CARTESIAN_POINT('Origin',(74.721079719791,66.9054073116123,212.));
#31434=CARTESIAN_POINT('',(74.721079719791,66.9054073116123,210.));
#31435=CARTESIAN_POINT('',(74.721079719791,66.9054073116123,210.));
#31436=CARTESIAN_POINT('',(74.721079719791,66.9054073116123,212.));
#31437=CARTESIAN_POINT('',(74.721079719791,66.9054073116123,212.));
#31438=CARTESIAN_POINT('',(74.721079719791,66.9054073116123,212.));
#31439=CARTESIAN_POINT('Origin',(72.2925272371593,65.7765304825996,212.));
#31440=CARTESIAN_POINT('',(72.2925272371593,65.7765304825996,210.));
#31441=CARTESIAN_POINT('',(72.2925272371593,65.7765304825996,210.));
#31442=CARTESIAN_POINT('',(72.2925272371593,65.7765304825996,212.));
#31443=CARTESIAN_POINT('',(72.2925272371593,65.7765304825996,212.));
#31444=CARTESIAN_POINT('',(72.2925272371593,65.7765304825996,212.));
#31445=CARTESIAN_POINT('Origin',(72.8815880880161,67.4244101244388,212.));
#31446=CARTESIAN_POINT('',(72.8815880880161,67.4244101244388,210.));
#31447=CARTESIAN_POINT('',(72.8815880880161,67.4244101244388,210.));
#31448=CARTESIAN_POINT('',(72.8815880880161,67.4244101244388,212.));
#31449=CARTESIAN_POINT('',(72.8815880880161,67.4244101244388,212.));
#31450=CARTESIAN_POINT('',(72.8815880880161,67.4244101244388,212.));
#31451=CARTESIAN_POINT('Origin',(70.3195608223071,66.6445086269775,212.));
#31452=CARTESIAN_POINT('',(70.3195608223071,66.6445086269775,210.));
#31453=CARTESIAN_POINT('',(70.3195608223071,66.6445086269775,210.));
#31454=CARTESIAN_POINT('',(70.3195608223071,66.6445086269775,212.));
#31455=CARTESIAN_POINT('',(70.3195608223071,66.6445086269775,212.));
#31456=CARTESIAN_POINT('',(70.3195608223071,66.6445086269775,212.));
#31457=CARTESIAN_POINT('Origin',(71.1322294932201,68.1943697921522,212.));
#31458=CARTESIAN_POINT('',(71.1322294932201,68.1943697921522,210.));
#31459=CARTESIAN_POINT('',(71.1322294932201,68.1943697921522,210.));
#31460=CARTESIAN_POINT('',(71.1322294932201,68.1943697921522,212.));
#31461=CARTESIAN_POINT('',(71.1322294932201,68.1943697921522,212.));
#31462=CARTESIAN_POINT('',(71.1322294932201,68.1943697921522,212.));
#31463=CARTESIAN_POINT('Origin',(68.4865943908981,67.7786235217654,212.));
#31464=CARTESIAN_POINT('',(68.4865943908981,67.7786235217654,210.));
#31465=CARTESIAN_POINT('',(68.4865943908981,67.7786235217654,210.));
#31466=CARTESIAN_POINT('',(68.4865943908981,67.7786235217654,212.));
#31467=CARTESIAN_POINT('',(68.4865943908981,67.7786235217654,212.));
#31468=CARTESIAN_POINT('',(68.4865943908981,67.7786235217654,212.));
#31469=CARTESIAN_POINT('Origin',(69.5070532105848,69.2002999256365,212.));
#31470=CARTESIAN_POINT('',(69.5070532105848,69.2002999256365,210.));
#31471=CARTESIAN_POINT('',(69.5070532105848,69.2002999256365,210.));
#31472=CARTESIAN_POINT('',(69.5070532105848,69.2002999256365,212.));
#31473=CARTESIAN_POINT('',(69.5070532105848,69.2002999256365,212.));
#31474=CARTESIAN_POINT('',(69.5070532105848,69.2002999256365,212.));
#31475=CARTESIAN_POINT('Origin',(66.8293045495512,69.156800910573,212.));
#31476=CARTESIAN_POINT('',(66.8293045495512,69.156800910573,210.));
#31477=CARTESIAN_POINT('',(66.8293045495512,69.156800910573,210.));
#31478=CARTESIAN_POINT('',(66.8293045495512,69.156800910573,212.));
#31479=CARTESIAN_POINT('',(66.8293045495512,69.156800910573,212.));
#31480=CARTESIAN_POINT('',(66.8293045495512,69.156800910573,212.));
#31481=CARTESIAN_POINT('Origin',(68.0376914478412,70.422621239072,212.));
#31482=CARTESIAN_POINT('',(68.0376914478412,70.422621239072,210.));
#31483=CARTESIAN_POINT('',(68.0376914478412,70.422621239072,210.));
#31484=CARTESIAN_POINT('',(68.0376914478412,70.422621239072,212.));
#31485=CARTESIAN_POINT('',(68.0376914478412,70.422621239072,212.));
#31486=CARTESIAN_POINT('',(68.0376914478412,70.422621239072,212.));
#31487=CARTESIAN_POINT('Origin',(65.379948559889,70.7522161381807,212.));
#31488=CARTESIAN_POINT('',(65.379948559889,70.7522161381807,210.));
#31489=CARTESIAN_POINT('',(65.379948559889,70.7522161381807,210.));
#31490=CARTESIAN_POINT('',(65.379948559889,70.7522161381807,212.));
#31491=CARTESIAN_POINT('',(65.379948559889,70.7522161381807,212.));
#31492=CARTESIAN_POINT('',(65.379948559889,70.7522161381807,212.));
#31493=CARTESIAN_POINT('Origin',(66.7527436603267,71.8375426384627,212.));
#31494=CARTESIAN_POINT('',(66.7527436603267,71.8375426384627,210.));
#31495=CARTESIAN_POINT('',(66.7527436603267,71.8375426384627,210.));
#31496=CARTESIAN_POINT('',(66.7527436603267,71.8375426384627,212.));
#31497=CARTESIAN_POINT('',(66.7527436603267,71.8375426384627,212.));
#31498=CARTESIAN_POINT('',(66.7527436603267,71.8375426384627,212.));
#31499=CARTESIAN_POINT('Origin',(64.1667364876323,72.533816261941,212.));
#31500=CARTESIAN_POINT('',(64.1667364876323,72.533816261941,210.));
#31501=CARTESIAN_POINT('',(64.1667364876323,72.533816261941,210.));
#31502=CARTESIAN_POINT('',(64.1667364876323,72.533816261941,212.));
#31503=CARTESIAN_POINT('',(64.1667364876323,72.533816261941,212.));
#31504=CARTESIAN_POINT('',(64.1667364876323,72.533816261941,212.));
#31505=CARTESIAN_POINT('Origin',(65.677219895119,73.4175242882186,212.));
#31506=CARTESIAN_POINT('',(65.677219895119,73.4175242882186,210.));
#31507=CARTESIAN_POINT('',(65.677219895119,73.4175242882186,210.));
#31508=CARTESIAN_POINT('',(65.677219895119,73.4175242882186,212.));
#31509=CARTESIAN_POINT('',(65.677219895119,73.4175242882186,212.));
#31510=CARTESIAN_POINT('',(65.677219895119,73.4175242882186,212.));
#31511=CARTESIAN_POINT('Origin',(63.2132821257592,74.466924461985,212.));
#31512=CARTESIAN_POINT('',(63.2132821257592,74.466924461985,210.));
#31513=CARTESIAN_POINT('',(63.2132821257592,74.466924461985,210.));
#31514=CARTESIAN_POINT('',(63.2132821257592,74.466924461985,212.));
#31515=CARTESIAN_POINT('',(63.2132821257592,74.466924461985,212.));
#31516=CARTESIAN_POINT('',(63.2132821257592,74.466924461985,212.));
#31517=CARTESIAN_POINT('Origin',(64.8320539989176,75.1318136427297,212.));
#31518=CARTESIAN_POINT('',(64.8320539989176,75.1318136427297,210.));
#31519=CARTESIAN_POINT('',(64.8320539989176,75.1318136427297,210.));
#31520=CARTESIAN_POINT('',(64.8320539989176,75.1318136427297,212.));
#31521=CARTESIAN_POINT('',(64.8320539989176,75.1318136427297,212.));
#31522=CARTESIAN_POINT('',(64.8320539989176,75.1318136427297,212.));
#31523=CARTESIAN_POINT('Origin',(62.5381433788854,76.5139149860768,212.));
#31524=CARTESIAN_POINT('',(62.5381433788854,76.5139149860768,210.));
#31525=CARTESIAN_POINT('',(62.5381433788854,76.5139149860768,210.));
#31526=CARTESIAN_POINT('',(62.5381433788854,76.5139149860768,212.));
#31527=CARTESIAN_POINT('',(62.5381433788854,76.5139149860768,212.));
#31528=CARTESIAN_POINT('',(62.5381433788854,76.5139149860768,212.));
#31529=CARTESIAN_POINT('Origin',(64.2336961645301,76.9470440096857,212.));
#31530=CARTESIAN_POINT('',(64.2336961645301,76.9470440096857,210.));
#31531=CARTESIAN_POINT('',(64.2336961645301,76.9470440096857,210.));
#31532=CARTESIAN_POINT('',(64.2336961645301,76.9470440096857,212.));
#31533=CARTESIAN_POINT('',(64.2336961645301,76.9470440096857,212.));
#31534=CARTESIAN_POINT('',(64.2336961645301,76.9470440096857,212.));
#31535=CARTESIAN_POINT('Origin',(62.1544610547598,78.6349454920823,212.));
#31536=CARTESIAN_POINT('',(62.1544610547598,78.6349454920823,210.));
#31537=CARTESIAN_POINT('',(62.1544610547598,78.6349454920823,210.));
#31538=CARTESIAN_POINT('',(62.1544610547598,78.6349454920823,212.));
#31539=CARTESIAN_POINT('',(62.1544610547598,78.6349454920823,212.));
#31540=CARTESIAN_POINT('',(62.1544610547598,78.6349454920823,212.));
#31541=CARTESIAN_POINT('Origin',(63.893792746581,78.8278839947877,212.));
#31542=CARTESIAN_POINT('',(63.893792746581,78.8278839947877,210.));
#31543=CARTESIAN_POINT('',(63.893792746581,78.8278839947877,210.));
#31544=CARTESIAN_POINT('',(63.893792746581,78.8278839947877,212.));
#31545=CARTESIAN_POINT('',(63.893792746581,78.8278839947877,212.));
#31546=CARTESIAN_POINT('',(63.893792746581,78.8278839947877,212.));
#31547=CARTESIAN_POINT('Origin',(62.0697030933893,80.7887325338384,212.));
#31548=CARTESIAN_POINT('',(62.0697030933893,80.7887325338384,210.));
#31549=CARTESIAN_POINT('',(62.0697030933893,80.7887325338384,210.));
#31550=CARTESIAN_POINT('',(62.0697030933893,80.7887325338384,212.));
#31551=CARTESIAN_POINT('',(62.0697030933893,80.7887325338384,212.));
#31552=CARTESIAN_POINT('',(62.0697030933893,80.7887325338384,212.));
#31553=CARTESIAN_POINT('Origin',(63.8189595784662,80.7377251871495,212.));
#31554=CARTESIAN_POINT('',(63.8189595784662,80.7377251871495,210.));
#31555=CARTESIAN_POINT('',(63.8189595784662,80.7377251871495,210.));
#31556=CARTESIAN_POINT('',(63.8189595784662,80.7377251871495,212.));
#31557=CARTESIAN_POINT('',(63.8189595784662,80.7377251871495,212.));
#31558=CARTESIAN_POINT('',(63.8189595784662,80.7377251871495,212.));
#31559=CARTESIAN_POINT('Origin',(62.2855192120812,82.9333550964738,212.));
#31560=CARTESIAN_POINT('',(62.2855192120812,82.9333550964738,210.));
#31561=CARTESIAN_POINT('',(62.2855192120812,82.9333550964738,210.));
#31562=CARTESIAN_POINT('',(62.2855192120812,82.9333550964738,212.));
#31563=CARTESIAN_POINT('',(62.2855192120812,82.9333550964738,212.));
#31564=CARTESIAN_POINT('',(62.2855192120812,82.9333550964738,212.));
#31565=CARTESIAN_POINT('Origin',(64.0106532026816,82.6393947003739,212.));
#31566=CARTESIAN_POINT('',(64.0106532026816,82.6393947003739,210.));
#31567=CARTESIAN_POINT('',(64.0106532026816,82.6393947003739,210.));
#31568=CARTESIAN_POINT('',(64.0106532026816,82.6393947003739,212.));
#31569=CARTESIAN_POINT('',(64.0106532026816,82.6393947003739,212.));
#31570=CARTESIAN_POINT('',(64.0106532026816,82.6393947003739,212.));
#31571=CARTESIAN_POINT('Origin',(62.7977087955725,85.0270705412788,212.));
#31572=CARTESIAN_POINT('',(62.7977087955725,85.0270705412788,210.));
#31573=CARTESIAN_POINT('',(62.7977087955725,85.0270705412788,210.));
#31574=CARTESIAN_POINT('',(62.7977087955725,85.0270705412788,212.));
#31575=CARTESIAN_POINT('',(62.7977087955725,85.0270705412788,212.));
#31576=CARTESIAN_POINT('',(62.7977087955725,85.0270705412788,212.));
#31577=CARTESIAN_POINT('Origin',(64.4651425208801,84.495878700503,212.));
#31578=CARTESIAN_POINT('',(64.4651425208801,84.495878700503,210.));
#31579=CARTESIAN_POINT('',(64.4651425208801,84.495878700503,210.));
#31580=CARTESIAN_POINT('',(64.4651425208801,84.495878700503,212.));
#31581=CARTESIAN_POINT('',(64.4651425208801,84.495878700503,212.));
#31582=CARTESIAN_POINT('',(64.4651425208801,84.495878700503,212.));
#31583=CARTESIAN_POINT('Origin',(63.5963026562275,87.0291270786864,212.));
#31584=CARTESIAN_POINT('',(63.5963026562275,87.0291270786864,210.));
#31585=CARTESIAN_POINT('',(63.5963026562275,87.0291270786864,210.));
#31586=CARTESIAN_POINT('',(63.5963026562275,87.0291270786864,212.));
#31587=CARTESIAN_POINT('',(63.5963026562275,87.0291270786864,212.));
#31588=CARTESIAN_POINT('',(63.5963026562275,87.0291270786864,212.));
#31589=CARTESIAN_POINT('Origin',(65.173581415457,86.2710428381936,212.));
#31590=CARTESIAN_POINT('',(65.173581415457,86.2710428381936,210.));
#31591=CARTESIAN_POINT('',(65.173581415457,86.2710428381936,210.));
#31592=CARTESIAN_POINT('',(65.173581415457,86.2710428381936,212.));
#31593=CARTESIAN_POINT('',(65.173581415457,86.2710428381936,212.));
#31594=CARTESIAN_POINT('',(65.173581415457,86.2710428381936,212.));
#31595=CARTESIAN_POINT('Origin',(64.6657570729356,88.9005569555014,212.));
#31596=CARTESIAN_POINT('',(64.6657570729356,88.9005569555014,210.));
#31597=CARTESIAN_POINT('',(64.6657570729356,88.9005569555014,210.));
#31598=CARTESIAN_POINT('',(64.6657570729356,88.9005569555014,212.));
#31599=CARTESIAN_POINT('',(64.6657570729356,88.9005569555014,212.));
#31600=CARTESIAN_POINT('',(64.6657570729356,88.9005569555014,212.));
#31601=CARTESIAN_POINT('Origin',(66.1221809291665,87.9303355627247,212.));
#31602=CARTESIAN_POINT('',(66.1221809291665,87.9303355627247,210.));
#31603=CARTESIAN_POINT('',(66.1221809291665,87.9303355627247,210.));
#31604=CARTESIAN_POINT('',(66.1221809291665,87.9303355627247,212.));
#31605=CARTESIAN_POINT('',(66.1221809291665,87.9303355627247,212.));
#31606=CARTESIAN_POINT('',(66.1221809291665,87.9303355627247,212.));
#31607=CARTESIAN_POINT('Origin',(65.9852563319619,90.6049349178915,212.));
#31608=CARTESIAN_POINT('',(65.9852563319619,90.6049349178915,210.));
#31609=CARTESIAN_POINT('',(65.9852563319619,90.6049349178915,210.));
#31610=CARTESIAN_POINT('',(65.9852563319619,90.6049349178915,212.));
#31611=CARTESIAN_POINT('',(65.9852563319619,90.6049349178915,212.));
#31612=CARTESIAN_POINT('',(65.9852563319619,90.6049349178915,212.));
#31613=CARTESIAN_POINT('Origin',(67.2924776514903,89.441460628631,212.));
#31614=CARTESIAN_POINT('',(67.2924776514903,89.441460628631,210.));
#31615=CARTESIAN_POINT('',(67.2924776514903,89.441460628631,210.));
#31616=CARTESIAN_POINT('',(67.2924776514903,89.441460628631,212.));
#31617=CARTESIAN_POINT('',(67.2924776514903,89.441460628631,212.));
#31618=CARTESIAN_POINT('',(67.2924776514903,89.441460628631,212.));
#31619=CARTESIAN_POINT('Origin',(67.5291178811376,92.1090871875201,212.));
#31620=CARTESIAN_POINT('',(67.5291178811376,92.1090871875201,210.));
#31621=CARTESIAN_POINT('',(67.5291178811376,92.1090871875201,210.));
#31622=CARTESIAN_POINT('',(67.5291178811376,92.1090871875201,212.));
#31623=CARTESIAN_POINT('',(67.5291178811376,92.1090871875201,212.));
#31624=CARTESIAN_POINT('',(67.5291178811376,92.1090871875201,212.));
#31625=CARTESIAN_POINT('Origin',(68.6616930879211,90.7750057053837,212.));
#31626=CARTESIAN_POINT('',(68.6616930879211,90.7750057053837,210.));
#31627=CARTESIAN_POINT('',(68.6616930879211,90.7750057053837,210.));
#31628=CARTESIAN_POINT('',(68.6616930879211,90.7750057053837,212.));
#31629=CARTESIAN_POINT('',(68.6616930879211,90.7750057053837,212.));
#31630=CARTESIAN_POINT('',(68.6616930879211,90.7750057053837,212.));
#31631=CARTESIAN_POINT('Origin',(69.2672922115245,93.3837371514067,212.));
#31632=CARTESIAN_POINT('',(69.2672922115245,93.3837371514067,210.));
#31633=CARTESIAN_POINT('',(69.2672922115245,93.3837371514067,210.));
#31634=CARTESIAN_POINT('',(69.2672922115245,93.3837371514067,212.));
#31635=CARTESIAN_POINT('',(69.2672922115245,93.3837371514067,212.));
#31636=CARTESIAN_POINT('',(69.2672922115245,93.3837371514067,212.));
#31637=CARTESIAN_POINT('Origin',(70.2031770174483,91.905014854949,212.));
#31638=CARTESIAN_POINT('',(70.2031770174483,91.905014854949,210.));
#31639=CARTESIAN_POINT('',(70.2031770174483,91.905014854949,210.));
#31640=CARTESIAN_POINT('',(70.2031770174483,91.905014854949,212.));
#31641=CARTESIAN_POINT('',(70.2031770174483,91.905014854949,212.));
#31642=CARTESIAN_POINT('',(70.2031770174483,91.905014854949,212.));
#31643=CARTESIAN_POINT('Origin',(71.1659477369257,94.404075197897,212.));
#31644=CARTESIAN_POINT('',(71.1659477369257,94.404075197897,210.));
#31645=CARTESIAN_POINT('',(71.1659477369257,94.404075197897,210.));
#31646=CARTESIAN_POINT('',(71.1659477369257,94.404075197897,212.));
#31647=CARTESIAN_POINT('',(71.1659477369257,94.404075197897,212.));
#31648=CARTESIAN_POINT('',(71.1659477369257,94.404075197897,212.));
#31649=CARTESIAN_POINT('Origin',(71.8869262087956,92.809493734597,212.));
#31650=CARTESIAN_POINT('',(71.8869262087956,92.809493734597,210.));
#31651=CARTESIAN_POINT('',(71.8869262087956,92.809493734597,210.));
#31652=CARTESIAN_POINT('',(71.8869262087956,92.809493734597,212.));
#31653=CARTESIAN_POINT('',(71.8869262087956,92.809493734597,212.));
#31654=CARTESIAN_POINT('',(71.8869262087956,92.809493734597,212.));
#31655=CARTESIAN_POINT('Origin',(73.1881292872278,95.1502416075335,212.));
#31656=CARTESIAN_POINT('',(73.1881292872279,95.1502416075335,210.));
#31657=CARTESIAN_POINT('',(73.1881292872279,95.1502416075335,210.));
#31658=CARTESIAN_POINT('',(73.1881292872278,95.1502416075335,212.));
#31659=CARTESIAN_POINT('',(73.1881292872278,95.1502416075335,212.));
#31660=CARTESIAN_POINT('',(73.1881292872278,95.1502416075335,212.));
#31661=CARTESIAN_POINT('Origin',(73.6801683991898,93.4708376917647,212.));
#31662=CARTESIAN_POINT('',(73.6801683991898,93.4708376917647,210.));
#31663=CARTESIAN_POINT('',(73.6801683991898,93.4708376917647,210.));
#31664=CARTESIAN_POINT('',(73.6801683991898,93.4708376917647,212.));
#31665=CARTESIAN_POINT('',(73.6801683991898,93.4708376917647,212.));
#31666=CARTESIAN_POINT('',(73.6801683991898,93.4708376917647,212.));
#31667=CARTESIAN_POINT('Origin',(75.2944773987517,95.6077130999043,212.));
#31668=CARTESIAN_POINT('',(75.2944773987517,95.6077130999043,210.));
#31669=CARTESIAN_POINT('',(75.2944773987517,95.6077130999043,210.));
#31670=CARTESIAN_POINT('',(75.2944773987517,95.6077130999043,212.));
#31671=CARTESIAN_POINT('',(75.2944773987517,95.6077130999043,212.));
#31672=CARTESIAN_POINT('',(75.2944773987517,95.6077130999043,212.));
#31673=CARTESIAN_POINT('Origin',(75.5480001691776,93.8761744185935,212.));
#31674=CARTESIAN_POINT('',(75.5480001691776,93.8761744185935,210.));
#31675=CARTESIAN_POINT('',(75.5480001691776,93.8761744185935,210.));
#31676=CARTESIAN_POINT('',(75.5480001691776,93.8761744185935,212.));
#31677=CARTESIAN_POINT('',(75.5480001691776,93.8761744185935,212.));
#31678=CARTESIAN_POINT('',(75.5480001691776,93.8761744185935,212.));
#31679=CARTESIAN_POINT('Origin',(77.443994401442,95.7675855127764,212.));
#31680=CARTESIAN_POINT('',(77.443994401442,95.7675855127764,210.));
#31681=CARTESIAN_POINT('',(77.443994401442,95.7675855127764,210.));
#31682=CARTESIAN_POINT('',(77.443994401442,95.7675855127764,212.));
#31683=CARTESIAN_POINT('',(77.443994401442,95.7675855127764,212.));
#31684=CARTESIAN_POINT('',(77.443994401442,95.7675855127764,212.));
#31685=CARTESIAN_POINT('Origin',(77.4540662979833,94.0176144967593,212.));
#31686=CARTESIAN_POINT('',(77.4540662979833,94.0176144967593,210.));
#31687=CARTESIAN_POINT('',(77.4540662979833,94.0176144967593,210.));
#31688=CARTESIAN_POINT('',(77.4540662979833,94.0176144967593,212.));
#31689=CARTESIAN_POINT('',(77.4540662979833,94.0176144967593,212.));
#31690=CARTESIAN_POINT('',(77.4540662979833,94.0176144967593,212.));
#31691=CARTESIAN_POINT('Origin',(79.5948423918807,95.6267471114856,212.));
#31692=CARTESIAN_POINT('',(79.5948423918807,95.6267471114856,210.));
#31693=CARTESIAN_POINT('',(79.5948423918807,95.6267471114856,210.));
#31694=CARTESIAN_POINT('',(79.5948423918807,95.6267471114856,212.));
#31695=CARTESIAN_POINT('',(79.5948423918807,95.6267471114856,212.));
#31696=CARTESIAN_POINT('',(79.5948423918807,95.6267471114856,212.));
#31697=CARTESIAN_POINT('Origin',(79.3612673765278,93.8924049560264,212.));
#31698=CARTESIAN_POINT('',(79.3612673765278,93.8924049560264,210.));
#31699=CARTESIAN_POINT('',(79.3612673765278,93.8924049560264,210.));
#31700=CARTESIAN_POINT('',(79.3612673765278,93.8924049560264,212.));
#31701=CARTESIAN_POINT('',(79.3612673765278,93.8924049560264,212.));
#31702=CARTESIAN_POINT('',(79.3612673765278,93.8924049560264,212.));
#31703=CARTESIAN_POINT('Origin',(81.7051575604872,95.1879391553116,212.));
#31704=CARTESIAN_POINT('',(81.7051575604872,95.1879391553116,210.));
#31705=CARTESIAN_POINT('',(81.7051575604872,95.1879391553116,210.));
#31706=CARTESIAN_POINT('',(81.7051575604872,95.1879391553116,212.));
#31707=CARTESIAN_POINT('',(81.7051575604872,95.1879391553116,212.));
#31708=CARTESIAN_POINT('',(81.7051575604872,95.1879391553116,212.));
#31709=CARTESIAN_POINT('Origin',(81.2324819052264,93.5029828576814,212.));
#31710=CARTESIAN_POINT('',(81.2324819052264,93.5029828576814,210.));
#31711=CARTESIAN_POINT('',(81.2324819052264,93.5029828576814,210.));
#31712=CARTESIAN_POINT('',(81.2324819052264,93.5029828576814,212.));
#31713=CARTESIAN_POINT('',(81.2324819052264,93.5029828576814,212.));
#31714=CARTESIAN_POINT('',(81.2324819052264,93.5029828576814,212.));
#31715=CARTESIAN_POINT('Origin',(83.7338650229525,94.4597025419847,212.));
#31716=CARTESIAN_POINT('',(83.7338650229525,94.4597025419847,210.));
#31717=CARTESIAN_POINT('',(83.7338650229525,94.4597025419847,210.));
#31718=CARTESIAN_POINT('',(83.7338650229525,94.4597025419847,212.));
#31719=CARTESIAN_POINT('',(83.7338650229525,94.4597025419847,212.));
#31720=CARTESIAN_POINT('',(83.7338650229525,94.4597025419847,212.));
#31721=CARTESIAN_POINT('Origin',(83.0312888217528,92.8569278599075,212.));
#31722=CARTESIAN_POINT('',(83.0312888217528,92.8569278599075,210.));
#31723=CARTESIAN_POINT('',(83.0312888217528,92.8569278599075,210.));
#31724=CARTESIAN_POINT('',(83.0312888217528,92.8569278599075,212.));
#31725=CARTESIAN_POINT('',(83.0312888217528,92.8569278599075,212.));
#31726=CARTESIAN_POINT('',(83.0312888217528,92.8569278599075,212.));
#31727=CARTESIAN_POINT('Origin',(85.6414782961402,93.4562115688265,212.));
#31728=CARTESIAN_POINT('',(85.6414782961402,93.4562115688265,210.));
#31729=CARTESIAN_POINT('',(85.6414782961402,93.4562115688265,210.));
#31730=CARTESIAN_POINT('',(85.6414782961402,93.4562115688265,212.));
#31731=CARTESIAN_POINT('',(85.6414782961402,93.4562115688265,212.));
#31732=CARTESIAN_POINT('',(85.6414782961402,93.4562115688265,212.));
#31733=CARTESIAN_POINT('Origin',(84.7226763955895,91.9668146883597,212.));
#31734=CARTESIAN_POINT('',(84.7226763955895,91.9668146883597,210.));
#31735=CARTESIAN_POINT('',(84.7226763955895,91.9668146883597,210.));
#31736=CARTESIAN_POINT('',(84.7226763955895,91.9668146883597,212.));
#31737=CARTESIAN_POINT('',(84.7226763955895,91.9668146883597,212.));
#31738=CARTESIAN_POINT('',(84.7226763955895,91.9668146883597,212.));
#31739=CARTESIAN_POINT('Origin',(87.3908678575658,92.1969980461754,212.));
#31740=CARTESIAN_POINT('',(87.3908678575658,92.1969980461754,210.));
#31741=CARTESIAN_POINT('',(87.3908678575658,92.1969980461754,210.));
#31742=CARTESIAN_POINT('',(87.3908678575658,92.1969980461754,212.));
#31743=CARTESIAN_POINT('',(87.3908678575658,92.1969980461754,212.));
#31744=CARTESIAN_POINT('',(87.3908678575658,92.1969980461754,212.));
#31745=CARTESIAN_POINT('Origin',(86.2737236915365,90.8499683834334,212.));
#31746=CARTESIAN_POINT('',(86.2737236915365,90.8499683834334,210.));
#31747=CARTESIAN_POINT('',(86.2737236915365,90.8499683834334,210.));
#31748=CARTESIAN_POINT('',(86.2737236915365,90.8499683834334,212.));
#31749=CARTESIAN_POINT('',(86.2737236915365,90.8499683834334,212.));
#31750=CARTESIAN_POINT('',(86.2737236915365,90.8499683834334,212.));
#31751=CARTESIAN_POINT('Origin',(88.9479838293171,90.7065711329157,212.));
#31752=CARTESIAN_POINT('',(88.9479838293171,90.7065711329157,210.));
#31753=CARTESIAN_POINT('',(88.9479838293171,90.7065711329157,210.));
#31754=CARTESIAN_POINT('',(88.9479838293171,90.7065711329157,212.));
#31755=CARTESIAN_POINT('',(88.9479838293171,90.7065711329157,212.));
#31756=CARTESIAN_POINT('',(88.9479838293171,90.7065711329157,212.));
#31757=CARTESIAN_POINT('Origin',(87.6542413382684,89.5281270880603,212.));
#31758=CARTESIAN_POINT('',(87.6542413382684,89.5281270880603,210.));
#31759=CARTESIAN_POINT('',(87.6542413382684,89.5281270880603,210.));
#31760=CARTESIAN_POINT('',(87.6542413382684,89.5281270880603,212.));
#31761=CARTESIAN_POINT('',(87.6542413382684,89.5281270880603,212.));
#31762=CARTESIAN_POINT('',(87.6542413382684,89.5281270880603,212.));
#31763=CARTESIAN_POINT('Origin',(90.2825187201973,89.0139402935784,212.));
#31764=CARTESIAN_POINT('',(90.2825187201973,89.0139402935784,210.));
#31765=CARTESIAN_POINT('',(90.2825187201973,89.0139402935784,210.));
#31766=CARTESIAN_POINT('',(90.2825187201973,89.0139402935784,212.));
#31767=CARTESIAN_POINT('',(90.2825187201973,89.0139402935784,212.));
#31768=CARTESIAN_POINT('',(90.2825187201973,89.0139402935784,212.));
#31769=CARTESIAN_POINT('Origin',(88.8373591301071,88.0270189394825,212.));
#31770=CARTESIAN_POINT('',(88.8373591301071,88.0270189394825,210.));
#31771=CARTESIAN_POINT('',(88.8373591301071,88.0270189394825,210.));
#31772=CARTESIAN_POINT('',(88.8373591301071,88.0270189394825,212.));
#31773=CARTESIAN_POINT('',(88.8373591301071,88.0270189394825,212.));
#31774=CARTESIAN_POINT('',(88.8373591301071,88.0270189394825,212.));
#31775=CARTESIAN_POINT('Origin',(91.3684973265662,87.1520506621122,212.));
#31776=CARTESIAN_POINT('',(91.3684973265662,87.1520506621122,210.));
#31777=CARTESIAN_POINT('',(91.3684973265662,87.1520506621122,210.));
#31778=CARTESIAN_POINT('',(91.3684973265662,87.1520506621122,212.));
#31779=CARTESIAN_POINT('',(91.3684973265662,87.1520506621122,212.));
#31780=CARTESIAN_POINT('',(91.3684973265662,87.1520506621122,212.));
#31781=CARTESIAN_POINT('Origin',(89.8000490250111,86.3758613003269,212.));
#31782=CARTESIAN_POINT('',(89.8000490250111,86.3758613003269,210.));
#31783=CARTESIAN_POINT('',(89.8000490250111,86.3758613003269,210.));
#31784=CARTESIAN_POINT('',(89.8000490250111,86.3758613003269,212.));
#31785=CARTESIAN_POINT('',(89.8000490250111,86.3758613003269,212.));
#31786=CARTESIAN_POINT('',(89.8000490250111,86.3758613003269,212.));
#31787=CARTESIAN_POINT('Origin',(92.1847823101333,85.1571418023256,212.));
#31788=CARTESIAN_POINT('',(92.1847823101333,85.1571418023257,210.));
#31789=CARTESIAN_POINT('',(92.1847823101333,85.1571418023257,210.));
#31790=CARTESIAN_POINT('',(92.1847823101333,85.1571418023256,212.));
#31791=CARTESIAN_POINT('',(92.1847823101333,85.1571418023256,212.));
#31792=CARTESIAN_POINT('',(92.1847823101333,85.1571418023256,212.));
#31793=CARTESIAN_POINT('Origin',(90.5235733592194,84.6067920758757,212.));
#31794=CARTESIAN_POINT('',(90.5235733592194,84.6067920758757,210.));
#31795=CARTESIAN_POINT('',(90.5235733592194,84.6067920758757,210.));
#31796=CARTESIAN_POINT('',(90.5235733592194,84.6067920758757,212.));
#31797=CARTESIAN_POINT('',(90.5235733592194,84.6067920758757,212.));
#31798=CARTESIAN_POINT('',(90.5235733592194,84.6067920758757,212.));
#31799=CARTESIAN_POINT('Origin',(92.7154856122038,83.0680423459992,212.));
#31800=CARTESIAN_POINT('',(92.7154856122038,83.0680423459992,210.));
#31801=CARTESIAN_POINT('',(92.7154856122038,83.0680423459992,210.));
#31802=CARTESIAN_POINT('',(92.7154856122038,83.0680423459992,212.));
#31803=CARTESIAN_POINT('',(92.7154856122038,83.0680423459992,212.));
#31804=CARTESIAN_POINT('',(92.7154856122038,83.0680423459992,212.));
#31805=CARTESIAN_POINT('Origin',(90.9938495545636,82.7542441862965,212.));
#31806=CARTESIAN_POINT('',(90.9938495545636,82.7542441862965,210.));
#31807=CARTESIAN_POINT('',(90.9938495545636,82.7542441862965,210.));
#31808=CARTESIAN_POINT('',(90.9938495545636,82.7542441862965,212.));
#31809=CARTESIAN_POINT('',(90.9938495545636,82.7542441862965,212.));
#31810=CARTESIAN_POINT('',(90.9938495545636,82.7542441862965,212.));
#31811=CARTESIAN_POINT('Origin',(92.950277696669,80.9254142377348,212.));
#31812=CARTESIAN_POINT('',(92.950277696669,80.9254142377348,210.));
#31813=CARTESIAN_POINT('',(92.950277696669,80.9254142377348,210.));
#31814=CARTESIAN_POINT('',(92.950277696669,80.9254142377348,212.));
#31815=CARTESIAN_POINT('',(92.950277696669,80.9254142377348,212.));
#31816=CARTESIAN_POINT('',(92.950277696669,80.9254142377348,212.));
#31817=CARTESIAN_POINT('Origin',(91.2017242198324,80.8542753690178,212.));
#31818=CARTESIAN_POINT('',(91.2017242198324,80.8542753690178,210.));
#31819=CARTESIAN_POINT('',(91.2017242198324,80.8542753690178,210.));
#31820=CARTESIAN_POINT('',(91.2017242198324,80.8542753690178,212.));
#31821=CARTESIAN_POINT('',(91.2017242198324,80.8542753690178,212.));
#31822=CARTESIAN_POINT('',(91.2017242198324,80.8542753690178,212.));
#31823=CARTESIAN_POINT('Origin',(92.8845886026769,78.7709612964565,212.));
#31824=CARTESIAN_POINT('',(92.8845886026769,78.7709612964565,210.));
#31825=CARTESIAN_POINT('',(92.8845886026769,78.7709612964565,210.));
#31826=CARTESIAN_POINT('',(92.8845886026769,78.7709612964565,212.));
#31827=CARTESIAN_POINT('',(92.8845886026769,78.7709612964565,212.));
#31828=CARTESIAN_POINT('',(92.8845886026769,78.7709612964565,212.));
#31829=CARTESIAN_POINT('Origin',(91.1431513111203,78.9438663558855,212.));
#31830=CARTESIAN_POINT('',(91.1431513111203,78.9438663558855,210.));
#31831=CARTESIAN_POINT('',(91.1431513111203,78.9438663558855,210.));
#31832=CARTESIAN_POINT('',(91.1431513111203,78.9438663558855,212.));
#31833=CARTESIAN_POINT('',(91.1431513111203,78.9438663558855,212.));
#31834=CARTESIAN_POINT('',(91.1431513111203,78.9438663558855,212.));
#31835=CARTESIAN_POINT('Origin',(92.5196968937216,76.6466174980124,212.));
#31836=CARTESIAN_POINT('',(92.5196968937216,76.6466174980124,210.));
#31837=CARTESIAN_POINT('',(92.5196968937216,76.6466174980124,212.));
#31838=CARTESIAN_POINT('Origin',(77.215862801455,80.368869783441,212.));
#31839=CARTESIAN_POINT('Origin',(77.215862801455,80.368869783441,210.));
#31840=CARTESIAN_POINT('Origin',(77.215862801455,80.3688697834411,196.));
#31841=CARTESIAN_POINT('Origin',(77.215862801455,80.368869783441,200.));
#31842=CARTESIAN_POINT('',(76.2705288876953,76.4821817600082,200.));
#31843=CARTESIAN_POINT('Origin',(77.215862801455,80.368869783441,200.));
#31844=CARTESIAN_POINT('Origin',(77.215862801455,80.368869783441,210.));
#31845=CARTESIAN_POINT('',(76.2705288876953,76.4821817600082,210.));
#31846=CARTESIAN_POINT('Origin',(77.215862801455,80.368869783441,210.));
#31847=CARTESIAN_POINT('Origin',(77.215862801455,80.368869783441,212.));
#31848=CARTESIAN_POINT('',(76.2705288876953,76.4821817600082,198.1));
#31849=CARTESIAN_POINT('',(78.1611967152146,84.2555578068738,198.1));
#31850=CARTESIAN_POINT('Origin',(77.215862801455,80.368869783441,198.1));
#31851=CARTESIAN_POINT('Origin',(77.215862801455,80.368869783441,198.1));
#31852=CARTESIAN_POINT('',(76.2705288876953,76.4821817600082,212.));
#31853=CARTESIAN_POINT('Ctrl Pts',(76.8377292359511,78.8141945740679,198.312499998088));
#31854=CARTESIAN_POINT('Ctrl Pts',(77.7353213865851,78.5958790582346,198.370833331422));
#31855=CARTESIAN_POINT('Ctrl Pts',(78.3731842446541,79.2640589050045,198.429166664755));
#31856=CARTESIAN_POINT('Ctrl Pts',(79.011047102723,79.9322387517744,198.487499998088));
#31857=CARTESIAN_POINT('Ctrl Pts',(78.7513178101579,80.8187341143776,198.545833331422));
#31858=CARTESIAN_POINT('Ctrl Pts',(78.4915885175929,81.7052294769809,198.604166664755));
#31859=CARTESIAN_POINT('Ctrl Pts',(77.5939963669589,81.9235449928141,198.662499998088));
#31860=CARTESIAN_POINT('Ctrl Pts',(76.6964042163248,82.1418605086474,198.720833331422));
#31861=CARTESIAN_POINT('Ctrl Pts',(76.0585413582559,81.4736806618775,198.779166664755));
#31862=CARTESIAN_POINT('Ctrl Pts',(75.420678500187,80.8055008151076,198.837499998088));
#31863=CARTESIAN_POINT('Ctrl Pts',(75.6804077927521,79.9190054525044,198.895833331422));
#31864=CARTESIAN_POINT('Ctrl Pts',(75.9401370853171,79.0325100899012,198.954166664755));
#31865=CARTESIAN_POINT('Ctrl Pts',(76.8377292359511,78.8141945740679,199.012499998088));
#31866=CARTESIAN_POINT('Ctrl Pts',(77.7353213865851,78.5958790582346,199.070833331422));
#31867=CARTESIAN_POINT('Ctrl Pts',(78.3731842446541,79.2640589050045,199.129166664755));
#31868=CARTESIAN_POINT('Ctrl Pts',(79.011047102723,79.9322387517744,199.187499998088));
#31869=CARTESIAN_POINT('Ctrl Pts',(78.7513178101579,80.8187341143776,199.245833331422));
#31870=CARTESIAN_POINT('Ctrl Pts',(78.4915885175929,81.7052294769809,199.304166664755));
#31871=CARTESIAN_POINT('Ctrl Pts',(77.5939963669589,81.9235449928141,199.362499998088));
#31872=CARTESIAN_POINT('Ctrl Pts',(76.6964042163248,82.1418605086474,199.420833331422));
#31873=CARTESIAN_POINT('Ctrl Pts',(76.0585413582559,81.4736806618775,199.479166664755));
#31874=CARTESIAN_POINT('Ctrl Pts',(75.420678500187,80.8055008151076,199.537499998088));
#31875=CARTESIAN_POINT('Ctrl Pts',(75.6804077927521,79.9190054525044,199.595833331422));
#31876=CARTESIAN_POINT('Ctrl Pts',(75.9401370853171,79.0325100899012,199.654166664755));
#31877=CARTESIAN_POINT('Ctrl Pts',(76.8377292359511,78.8141945740679,199.712499998088));
#31878=CARTESIAN_POINT('Ctrl Pts',(77.7353213865851,78.5958790582346,199.770833331422));
#31879=CARTESIAN_POINT('Ctrl Pts',(78.3731842446541,79.2640589050045,199.829166664755));
#31880=CARTESIAN_POINT('Ctrl Pts',(79.011047102723,79.9322387517744,199.887499998088));
#31881=CARTESIAN_POINT('Ctrl Pts',(78.7513178101579,80.8187341143776,199.945833331422));
#31882=CARTESIAN_POINT('Ctrl Pts',(78.4915885175929,81.7052294769809,200.004166664755));
#31883=CARTESIAN_POINT('Ctrl Pts',(77.5939963669589,81.9235449928141,200.062499998088));
#31884=CARTESIAN_POINT('Ctrl Pts',(76.6964042163248,82.1418605086474,200.120833331422));
#31885=CARTESIAN_POINT('Ctrl Pts',(76.0585413582559,81.4736806618775,200.179166664755));
#31886=CARTESIAN_POINT('Ctrl Pts',(75.420678500187,80.8055008151076,200.237499998088));
#31887=CARTESIAN_POINT('Ctrl Pts',(75.680407792752,79.9190054525044,200.295833331422));
#31888=CARTESIAN_POINT('Ctrl Pts',(75.9401370853171,79.0325100899012,200.354166664755));
#31889=CARTESIAN_POINT('Ctrl Pts',(76.8377292359511,78.8141945740679,200.412499998088));
#31890=CARTESIAN_POINT('Ctrl Pts',(77.7353213865851,78.5958790582346,200.470833331422));
#31891=CARTESIAN_POINT('Ctrl Pts',(78.3731842446541,79.2640589050045,200.529166664755));
#31892=CARTESIAN_POINT('Ctrl Pts',(79.011047102723,79.9322387517744,200.587499998088));
#31893=CARTESIAN_POINT('Ctrl Pts',(78.7513178101579,80.8187341143776,200.645833331422));
#31894=CARTESIAN_POINT('Ctrl Pts',(78.4915885175929,81.7052294769809,200.704166664755));
#31895=CARTESIAN_POINT('Ctrl Pts',(77.5939963669589,81.9235449928141,200.762499998088));
#31896=CARTESIAN_POINT('Ctrl Pts',(76.6964042163248,82.1418605086474,200.820833331422));
#31897=CARTESIAN_POINT('Ctrl Pts',(76.0585413582559,81.4736806618775,200.879166664755));
#31898=CARTESIAN_POINT('Ctrl Pts',(75.420678500187,80.8055008151076,200.937499998088));
#31899=CARTESIAN_POINT('Ctrl Pts',(75.680407792752,79.9190054525044,200.995833331422));
#31900=CARTESIAN_POINT('Ctrl Pts',(75.9401370853171,79.0325100899012,201.054166664755));
#31901=CARTESIAN_POINT('Ctrl Pts',(76.8377292359511,78.8141945740679,201.112499998088));
#31902=CARTESIAN_POINT('Ctrl Pts',(77.7353213865851,78.5958790582346,201.170833331422));
#31903=CARTESIAN_POINT('Ctrl Pts',(78.3731842446541,79.2640589050045,201.229166664755));
#31904=CARTESIAN_POINT('Ctrl Pts',(79.011047102723,79.9322387517744,201.287499998088));
#31905=CARTESIAN_POINT('Ctrl Pts',(78.7513178101579,80.8187341143776,201.345833331422));
#31906=CARTESIAN_POINT('Ctrl Pts',(78.4915885175929,81.7052294769809,201.404166664755));
#31907=CARTESIAN_POINT('Ctrl Pts',(77.5939963669589,81.9235449928141,201.462499998088));
#31908=CARTESIAN_POINT('Ctrl Pts',(76.6964042163248,82.1418605086474,201.520833331422));
#31909=CARTESIAN_POINT('Ctrl Pts',(76.0585413582559,81.4736806618775,201.579166664755));
#31910=CARTESIAN_POINT('Ctrl Pts',(75.420678500187,80.8055008151076,201.637499998088));
#31911=CARTESIAN_POINT('Ctrl Pts',(75.680407792752,79.9190054525044,201.695833331422));
#31912=CARTESIAN_POINT('Ctrl Pts',(75.9401370853171,79.0325100899012,201.754166664755));
#31913=CARTESIAN_POINT('Ctrl Pts',(76.8377292359511,78.8141945740679,201.812499998088));
#31914=CARTESIAN_POINT('Ctrl Pts',(77.7353213865851,78.5958790582346,201.870833331422));
#31915=CARTESIAN_POINT('Ctrl Pts',(78.3731842446541,79.2640589050045,201.929166664755));
#31916=CARTESIAN_POINT('Ctrl Pts',(79.011047102723,79.9322387517744,201.987499998088));
#31917=CARTESIAN_POINT('Ctrl Pts',(78.7513178101579,80.8187341143776,202.045833331422));
#31918=CARTESIAN_POINT('Ctrl Pts',(78.4915885175929,81.7052294769808,202.104166664755));
#31919=CARTESIAN_POINT('Ctrl Pts',(77.5939963669589,81.9235449928141,202.162499998088));
#31920=CARTESIAN_POINT('Ctrl Pts',(76.6964042163248,82.1418605086474,202.220833331422));
#31921=CARTESIAN_POINT('Ctrl Pts',(76.0585413582559,81.4736806618775,202.279166664755));
#31922=CARTESIAN_POINT('Ctrl Pts',(75.420678500187,80.8055008151076,202.337499998088));
#31923=CARTESIAN_POINT('Ctrl Pts',(75.680407792752,79.9190054525044,202.395833331422));
#31924=CARTESIAN_POINT('Ctrl Pts',(75.9401370853171,79.0325100899012,202.454166664755));
#31925=CARTESIAN_POINT('Ctrl Pts',(76.8377292359511,78.8141945740679,202.512499998088));
#31926=CARTESIAN_POINT('Ctrl Pts',(77.7353213865851,78.5958790582346,202.570833331422));
#31927=CARTESIAN_POINT('Ctrl Pts',(78.3731842446541,79.2640589050045,202.629166664755));
#31928=CARTESIAN_POINT('Ctrl Pts',(79.011047102723,79.9322387517744,202.687499998088));
#31929=CARTESIAN_POINT('Ctrl Pts',(78.7513178101579,80.8187341143776,202.745833331422));
#31930=CARTESIAN_POINT('Ctrl Pts',(78.4915885175929,81.7052294769808,202.804166664755));
#31931=CARTESIAN_POINT('Ctrl Pts',(77.5939963669589,81.9235449928141,202.862499998088));
#31932=CARTESIAN_POINT('Ctrl Pts',(76.6964042163248,82.1418605086474,202.920833331422));
#31933=CARTESIAN_POINT('Ctrl Pts',(76.0585413582559,81.4736806618775,202.979166664755));
#31934=CARTESIAN_POINT('Ctrl Pts',(75.420678500187,80.8055008151076,203.037499998088));
#31935=CARTESIAN_POINT('Ctrl Pts',(75.680407792752,79.9190054525044,203.095833331422));
#31936=CARTESIAN_POINT('Ctrl Pts',(75.9401370853171,79.0325100899012,203.154166664755));
#31937=CARTESIAN_POINT('Ctrl Pts',(76.8377292359511,78.8141945740679,203.212499998088));
#31938=CARTESIAN_POINT('Ctrl Pts',(77.7353213865851,78.5958790582346,203.270833331422));
#31939=CARTESIAN_POINT('Ctrl Pts',(78.3731842446541,79.2640589050045,203.329166664755));
#31940=CARTESIAN_POINT('Ctrl Pts',(79.011047102723,79.9322387517744,203.387499998088));
#31941=CARTESIAN_POINT('Ctrl Pts',(78.7513178101579,80.8187341143776,203.445833331422));
#31942=CARTESIAN_POINT('Ctrl Pts',(78.4915885175929,81.7052294769808,203.504166664755));
#31943=CARTESIAN_POINT('Ctrl Pts',(77.5939963669589,81.9235449928141,203.562499998088));
#31944=CARTESIAN_POINT('Ctrl Pts',(76.6964042163248,82.1418605086474,203.620833331422));
#31945=CARTESIAN_POINT('Ctrl Pts',(76.0585413582559,81.4736806618775,203.679166664755));
#31946=CARTESIAN_POINT('Ctrl Pts',(75.420678500187,80.8055008151076,203.737499998088));
#31947=CARTESIAN_POINT('Ctrl Pts',(75.680407792752,79.9190054525044,203.795833331422));
#31948=CARTESIAN_POINT('Ctrl Pts',(75.9401370853171,79.0325100899012,203.854166664755));
#31949=CARTESIAN_POINT('Ctrl Pts',(76.8377292359511,78.8141945740679,203.912499998088));
#31950=CARTESIAN_POINT('Ctrl Pts',(77.7353213865851,78.5958790582346,203.970833331422));
#31951=CARTESIAN_POINT('Ctrl Pts',(78.3731842446541,79.2640589050045,204.029166664755));
#31952=CARTESIAN_POINT('Ctrl Pts',(79.011047102723,79.9322387517744,204.087499998088));
#31953=CARTESIAN_POINT('Ctrl Pts',(78.7513178101579,80.8187341143776,204.145833331422));
#31954=CARTESIAN_POINT('Ctrl Pts',(78.4915885175929,81.7052294769808,204.204166664755));
#31955=CARTESIAN_POINT('Ctrl Pts',(77.5939963669589,81.9235449928141,204.262499998088));
#31956=CARTESIAN_POINT('Ctrl Pts',(76.6964042163248,82.1418605086474,204.320833331422));
#31957=CARTESIAN_POINT('Ctrl Pts',(76.0585413582559,81.4736806618775,204.379166664755));
#31958=CARTESIAN_POINT('Ctrl Pts',(75.420678500187,80.8055008151076,204.437499998088));
#31959=CARTESIAN_POINT('Ctrl Pts',(75.680407792752,79.9190054525044,204.495833331422));
#31960=CARTESIAN_POINT('Ctrl Pts',(75.9401370853171,79.0325100899012,204.554166664755));
#31961=CARTESIAN_POINT('Ctrl Pts',(76.8377292359511,78.8141945740679,204.612499998088));
#31962=CARTESIAN_POINT('Ctrl Pts',(77.7353213865851,78.5958790582346,204.670833331422));
#31963=CARTESIAN_POINT('Ctrl Pts',(78.3731842446541,79.2640589050045,204.729166664755));
#31964=CARTESIAN_POINT('Ctrl Pts',(79.011047102723,79.9322387517744,204.787499998088));
#31965=CARTESIAN_POINT('Ctrl Pts',(78.7513178101579,80.8187341143776,204.845833331422));
#31966=CARTESIAN_POINT('Ctrl Pts',(78.4915885175929,81.7052294769808,204.904166664755));
#31967=CARTESIAN_POINT('Ctrl Pts',(77.5939963669589,81.9235449928141,204.962499998088));
#31968=CARTESIAN_POINT('Ctrl Pts',(76.6964042163248,82.1418605086474,205.020833331422));
#31969=CARTESIAN_POINT('Ctrl Pts',(76.0585413582559,81.4736806618775,205.079166664755));
#31970=CARTESIAN_POINT('Ctrl Pts',(75.420678500187,80.8055008151076,205.137499998088));
#31971=CARTESIAN_POINT('Ctrl Pts',(75.680407792752,79.9190054525044,205.195833331422));
#31972=CARTESIAN_POINT('Ctrl Pts',(75.9401370853171,79.0325100899011,205.254166664755));
#31973=CARTESIAN_POINT('Ctrl Pts',(76.8377292359511,78.8141945740679,205.312499998088));
#31974=CARTESIAN_POINT('Ctrl Pts',(77.7353213865851,78.5958790582346,205.370833331422));
#31975=CARTESIAN_POINT('Ctrl Pts',(78.3731842446541,79.2640589050045,205.429166664755));
#31976=CARTESIAN_POINT('Ctrl Pts',(79.011047102723,79.9322387517744,205.487499998088));
#31977=CARTESIAN_POINT('Ctrl Pts',(78.7513178101579,80.8187341143776,205.545833331422));
#31978=CARTESIAN_POINT('Ctrl Pts',(78.4915885175928,81.7052294769808,205.604166664755));
#31979=CARTESIAN_POINT('Ctrl Pts',(77.5939963669589,81.9235449928141,205.662499998088));
#31980=CARTESIAN_POINT('Ctrl Pts',(76.6964042163248,82.1418605086474,205.720833331422));
#31981=CARTESIAN_POINT('Ctrl Pts',(76.0585413582559,81.4736806618775,205.779166664755));
#31982=CARTESIAN_POINT('Ctrl Pts',(75.420678500187,80.8055008151076,205.837499998088));
#31983=CARTESIAN_POINT('Ctrl Pts',(75.680407792752,79.9190054525044,205.895833331421));
#31984=CARTESIAN_POINT('Ctrl Pts',(75.9401370853171,79.0325100899011,205.954166664755));
#31985=CARTESIAN_POINT('Ctrl Pts',(76.8377292359511,78.8141945740679,206.012499998088));
#31986=CARTESIAN_POINT('Ctrl Pts',(77.7353213865851,78.5958790582346,206.070833331422));
#31987=CARTESIAN_POINT('Ctrl Pts',(78.3731842446541,79.2640589050045,206.129166664755));
#31988=CARTESIAN_POINT('Ctrl Pts',(79.011047102723,79.9322387517744,206.187499998088));
#31989=CARTESIAN_POINT('Ctrl Pts',(78.7513178101579,80.8187341143776,206.245833331422));
#31990=CARTESIAN_POINT('Ctrl Pts',(78.4915885175928,81.7052294769808,206.304166664755));
#31991=CARTESIAN_POINT('Ctrl Pts',(77.5939963669589,81.9235449928141,206.362499998088));
#31992=CARTESIAN_POINT('Ctrl Pts',(76.6964042163248,82.1418605086474,206.420833331422));
#31993=CARTESIAN_POINT('Ctrl Pts',(76.0585413582559,81.4736806618775,206.479166664755));
#31994=CARTESIAN_POINT('Ctrl Pts',(75.420678500187,80.8055008151076,206.537499998088));
#31995=CARTESIAN_POINT('Ctrl Pts',(75.680407792752,79.9190054525043,206.595833331422));
#31996=CARTESIAN_POINT('Ctrl Pts',(75.9401370853171,79.0325100899011,206.654166664755));
#31997=CARTESIAN_POINT('Ctrl Pts',(76.8377292359511,78.8141945740679,206.712499998088));
#31998=CARTESIAN_POINT('Ctrl Pts',(77.7353213865851,78.5958790582346,206.770833331422));
#31999=CARTESIAN_POINT('Ctrl Pts',(78.3731842446541,79.2640589050045,206.829166664755));
#32000=CARTESIAN_POINT('Ctrl Pts',(79.011047102723,79.9322387517744,206.887499998088));
#32001=CARTESIAN_POINT('Ctrl Pts',(78.7513178101579,80.8187341143776,206.945833331422));
#32002=CARTESIAN_POINT('Ctrl Pts',(78.4915885175928,81.7052294769808,207.004166664755));
#32003=CARTESIAN_POINT('Ctrl Pts',(77.5939963669589,81.9235449928141,207.062499998088));
#32004=CARTESIAN_POINT('Ctrl Pts',(76.6964042163248,82.1418605086474,207.120833331421));
#32005=CARTESIAN_POINT('Ctrl Pts',(76.0585413582559,81.4736806618775,207.179166664755));
#32006=CARTESIAN_POINT('Ctrl Pts',(75.420678500187,80.8055008151075,207.237499998088));
#32007=CARTESIAN_POINT('Ctrl Pts',(75.680407792752,79.9190054525043,207.295833331422));
#32008=CARTESIAN_POINT('Ctrl Pts',(75.9401370853171,79.0325100899011,207.354166664755));
#32009=CARTESIAN_POINT('Ctrl Pts',(76.8377292359511,78.8141945740679,207.412499998088));
#32010=CARTESIAN_POINT('Ctrl Pts',(77.7353213865851,78.5958790582346,207.470833331422));
#32011=CARTESIAN_POINT('Ctrl Pts',(78.3731842446541,79.2640589050045,207.529166664755));
#32012=CARTESIAN_POINT('Ctrl Pts',(79.011047102723,79.9322387517744,207.587499998088));
#32013=CARTESIAN_POINT('Ctrl Pts',(78.7513178101579,80.8187341143776,207.645833331422));
#32014=CARTESIAN_POINT('Ctrl Pts',(78.4915885175928,81.7052294769808,207.704166664755));
#32015=CARTESIAN_POINT('Ctrl Pts',(77.5939963669589,81.9235449928141,207.762499998088));
#32016=CARTESIAN_POINT('Ctrl Pts',(76.6964042163248,82.1418605086474,207.820833331422));
#32017=CARTESIAN_POINT('Ctrl Pts',(76.0585413582559,81.4736806618775,207.879166664755));
#32018=CARTESIAN_POINT('Ctrl Pts',(75.420678500187,80.8055008151075,207.937499998088));
#32019=CARTESIAN_POINT('Ctrl Pts',(75.680407792752,79.9190054525043,207.995833331422));
#32020=CARTESIAN_POINT('Ctrl Pts',(75.9401370853171,79.0325100899011,208.054166664755));
#32021=CARTESIAN_POINT('Ctrl Pts',(76.8377292359511,78.8141945740679,208.112499998088));
#32022=CARTESIAN_POINT('Ctrl Pts',(77.7353213865851,78.5958790582346,208.170833331422));
#32023=CARTESIAN_POINT('Ctrl Pts',(78.3731842446541,79.2640589050045,208.229166664755));
#32024=CARTESIAN_POINT('Ctrl Pts',(79.011047102723,79.9322387517744,208.287499998088));
#32025=CARTESIAN_POINT('Ctrl Pts',(78.7513178101579,80.8187341143776,208.345833331422));
#32026=CARTESIAN_POINT('Ctrl Pts',(78.4915885175928,81.7052294769808,208.404166664755));
#32027=CARTESIAN_POINT('Ctrl Pts',(77.5939963669589,81.9235449928141,208.462499998088));
#32028=CARTESIAN_POINT('Ctrl Pts',(76.6964042163248,82.1418605086474,208.520833331422));
#32029=CARTESIAN_POINT('Ctrl Pts',(76.0585413582559,81.4736806618775,208.579166664755));
#32030=CARTESIAN_POINT('Ctrl Pts',(75.420678500187,80.8055008151075,208.637499998088));
#32031=CARTESIAN_POINT('Ctrl Pts',(75.680407792752,79.9190054525043,208.695833331422));
#32032=CARTESIAN_POINT('Ctrl Pts',(75.9401370853171,79.0325100899011,208.754166664755));
#32033=CARTESIAN_POINT('Ctrl Pts',(76.8377292359511,78.8141945740679,208.812499998088));
#32034=CARTESIAN_POINT('Ctrl Pts',(77.7353213865851,78.5958790582346,208.870833331422));
#32035=CARTESIAN_POINT('Ctrl Pts',(78.3731842446541,79.2640589050045,208.929166664755));
#32036=CARTESIAN_POINT('Ctrl Pts',(79.011047102723,79.9322387517744,208.987499998088));
#32037=CARTESIAN_POINT('Ctrl Pts',(78.7513178101579,80.8187341143776,209.045833331422));
#32038=CARTESIAN_POINT('Ctrl Pts',(78.4915885175928,81.7052294769808,209.104166664755));
#32039=CARTESIAN_POINT('Ctrl Pts',(77.5939963669589,81.9235449928141,209.162499998088));
#32040=CARTESIAN_POINT('Ctrl Pts',(76.6964042163248,82.1418605086474,209.220833331422));
#32041=CARTESIAN_POINT('Ctrl Pts',(76.0585413582559,81.4736806618775,209.279166664755));
#32042=CARTESIAN_POINT('Ctrl Pts',(75.420678500187,80.8055008151075,209.337499998088));
#32043=CARTESIAN_POINT('Ctrl Pts',(75.680407792752,79.9190054525043,209.395833331422));
#32044=CARTESIAN_POINT('Ctrl Pts',(75.9401370853171,79.0325100899011,209.454166664755));
#32045=CARTESIAN_POINT('Ctrl Pts',(76.8377292359511,78.8141945740679,209.512499998088));
#32046=CARTESIAN_POINT('Ctrl Pts',(77.7353213865851,78.5958790582346,209.570833331422));
#32047=CARTESIAN_POINT('Ctrl Pts',(78.3731842446541,79.2640589050045,209.629166664755));
#32048=CARTESIAN_POINT('Ctrl Pts',(79.011047102723,79.9322387517744,209.687499998088));
#32049=CARTESIAN_POINT('Ctrl Pts',(78.7513178101579,80.8187341143776,209.745833331422));
#32050=CARTESIAN_POINT('Ctrl Pts',(78.4915885175928,81.7052294769808,209.804166664755));
#32051=CARTESIAN_POINT('Ctrl Pts',(77.5939963669589,81.9235449928141,209.862499998088));
#32052=CARTESIAN_POINT('Ctrl Pts',(76.6964042163248,82.1418605086474,209.920833331422));
#32053=CARTESIAN_POINT('Ctrl Pts',(76.0585413582559,81.4736806618775,209.979166664755));
#32054=CARTESIAN_POINT('Ctrl Pts',(75.420678500187,80.8055008151075,210.037499998088));
#32055=CARTESIAN_POINT('Ctrl Pts',(75.680407792752,79.9190054525043,210.095833331422));
#32056=CARTESIAN_POINT('Ctrl Pts',(75.9401370853171,79.0325100899011,210.154166664755));
#32057=CARTESIAN_POINT('Ctrl Pts',(76.8377292359511,78.8141945740679,210.212499998088));
#32058=CARTESIAN_POINT('Ctrl Pts',(77.7353213865851,78.5958790582346,210.270833331422));
#32059=CARTESIAN_POINT('Ctrl Pts',(78.3731842446541,79.2640589050045,210.329166664755));
#32060=CARTESIAN_POINT('Ctrl Pts',(79.011047102723,79.9322387517744,210.387499998088));
#32061=CARTESIAN_POINT('Ctrl Pts',(78.7513178101579,80.8187341143776,210.445833331422));
#32062=CARTESIAN_POINT('Ctrl Pts',(78.4915885175928,81.7052294769808,210.504166664755));
#32063=CARTESIAN_POINT('Ctrl Pts',(77.5939963669589,81.9235449928141,210.562499998088));
#32064=CARTESIAN_POINT('Ctrl Pts',(76.6964042163248,82.1418605086474,210.620833331422));
#32065=CARTESIAN_POINT('Ctrl Pts',(76.0585413582559,81.4736806618775,210.679166664755));
#32066=CARTESIAN_POINT('Ctrl Pts',(75.420678500187,80.8055008151075,210.737499998088));
#32067=CARTESIAN_POINT('Ctrl Pts',(75.680407792752,79.9190054525043,210.795833331422));
#32068=CARTESIAN_POINT('Ctrl Pts',(75.9401370853171,79.0325100899011,210.854166664755));
#32069=CARTESIAN_POINT('Ctrl Pts',(76.8377292359511,78.8141945740679,210.912499998088));
#32070=CARTESIAN_POINT('Ctrl Pts',(77.7353213865851,78.5958790582346,210.970833331422));
#32071=CARTESIAN_POINT('Ctrl Pts',(78.3731842446541,79.2640589050045,211.029166664755));
#32072=CARTESIAN_POINT('Ctrl Pts',(79.011047102723,79.9322387517744,211.087499998088));
#32073=CARTESIAN_POINT('Ctrl Pts',(78.7513178101579,80.8187341143776,211.145833331421));
#32074=CARTESIAN_POINT('Ctrl Pts',(78.4915885175928,81.7052294769808,211.204166664755));
#32075=CARTESIAN_POINT('Ctrl Pts',(77.5939963669589,81.9235449928141,211.262499998088));
#32076=CARTESIAN_POINT('Ctrl Pts',(76.6964042163248,82.1418605086474,211.320833331422));
#32077=CARTESIAN_POINT('Ctrl Pts',(76.0585413582559,81.4736806618775,211.379166664755));
#32078=CARTESIAN_POINT('Ctrl Pts',(75.420678500187,80.8055008151075,211.437499998088));
#32079=CARTESIAN_POINT('Ctrl Pts',(75.680407792752,79.9190054525043,211.495833331422));
#32080=CARTESIAN_POINT('Ctrl Pts',(75.9401370853171,79.0325100899011,211.554166664755));
#32081=CARTESIAN_POINT('Ctrl Pts',(76.8377292359511,78.8141945740679,211.612499998088));
#32082=CARTESIAN_POINT('Ctrl Pts',(77.7353213865851,78.5958790582346,211.670833331422));
#32083=CARTESIAN_POINT('Ctrl Pts',(78.3731842446541,79.2640589050045,211.729166664755));
#32084=CARTESIAN_POINT('Ctrl Pts',(79.011047102723,79.9322387517744,211.787499998088));
#32085=CARTESIAN_POINT('Ctrl Pts',(78.7513178101579,80.8187341143776,211.845833331422));
#32086=CARTESIAN_POINT('Ctrl Pts',(78.4915885175928,81.7052294769808,211.904166664755));
#32087=CARTESIAN_POINT('Ctrl Pts',(77.5939963669588,81.9235449928141,211.962499998088));
#32088=CARTESIAN_POINT('Ctrl Pts',(76.6964042163248,82.1418605086474,212.020833331422));
#32089=CARTESIAN_POINT('Ctrl Pts',(76.0585413582559,81.4736806618775,212.079166664755));
#32090=CARTESIAN_POINT('Ctrl Pts',(75.420678500187,80.8055008151075,212.137499998088));
#32091=CARTESIAN_POINT('Ctrl Pts',(75.680407792752,79.9190054525043,212.195833331422));
#32092=CARTESIAN_POINT('Ctrl Pts',(75.9401370853171,79.0325100899011,212.254166664755));
#32093=CARTESIAN_POINT('Ctrl Pts',(76.8377292359511,78.8141945740678,212.312499998088));
#32094=CARTESIAN_POINT('Ctrl Pts',(76.9272727088509,79.1823476029926,198.093749999044));
#32095=CARTESIAN_POINT('Ctrl Pts',(77.6123116091322,79.0157300353421,198.152083332377));
#32096=CARTESIAN_POINT('Ctrl Pts',(78.099126105575,79.5256823417411,198.210416665711));
#32097=CARTESIAN_POINT('Ctrl Pts',(78.5859406020177,80.0356346481401,198.268749999044));
#32098=CARTESIAN_POINT('Ctrl Pts',(78.3877161981791,80.7122045221895,198.327083332377));
#32099=CARTESIAN_POINT('Ctrl Pts',(78.1894917943405,81.388774396239,198.385416665711));
#32100=CARTESIAN_POINT('Ctrl Pts',(77.5044528940591,81.5553919638894,198.443749999044));
#32101=CARTESIAN_POINT('Ctrl Pts',(76.8194139937778,81.7220095315399,198.502083332377));
#32102=CARTESIAN_POINT('Ctrl Pts',(76.332599497335,81.2120572251409,198.560416665711));
#32103=CARTESIAN_POINT('Ctrl Pts',(75.8457850008923,80.702104918742,198.618749999044));
#32104=CARTESIAN_POINT('Ctrl Pts',(76.0440094047309,80.0255350446925,198.677083332377));
#32105=CARTESIAN_POINT('Ctrl Pts',(76.2422338085695,79.348965170643,198.735416665711));
#32106=CARTESIAN_POINT('Ctrl Pts',(76.9272727088509,79.1823476029926,198.793749999044));
#32107=CARTESIAN_POINT('Ctrl Pts',(77.6123116091322,79.0157300353421,198.852083332378));
#32108=CARTESIAN_POINT('Ctrl Pts',(78.099126105575,79.5256823417411,198.910416665711));
#32109=CARTESIAN_POINT('Ctrl Pts',(78.5859406020177,80.0356346481401,198.968749999044));
#32110=CARTESIAN_POINT('Ctrl Pts',(78.3877161981791,80.7122045221895,199.027083332377));
#32111=CARTESIAN_POINT('Ctrl Pts',(78.1894917943405,81.388774396239,199.085416665711));
#32112=CARTESIAN_POINT('Ctrl Pts',(77.5044528940591,81.5553919638894,199.143749999044));
#32113=CARTESIAN_POINT('Ctrl Pts',(76.8194139937778,81.7220095315399,199.202083332377));
#32114=CARTESIAN_POINT('Ctrl Pts',(76.332599497335,81.2120572251409,199.260416665711));
#32115=CARTESIAN_POINT('Ctrl Pts',(75.8457850008923,80.702104918742,199.318749999044));
#32116=CARTESIAN_POINT('Ctrl Pts',(76.0440094047309,80.0255350446925,199.377083332377));
#32117=CARTESIAN_POINT('Ctrl Pts',(76.2422338085695,79.348965170643,199.435416665711));
#32118=CARTESIAN_POINT('Ctrl Pts',(76.9272727088509,79.1823476029926,199.493749999044));
#32119=CARTESIAN_POINT('Ctrl Pts',(77.6123116091322,79.0157300353421,199.552083332377));
#32120=CARTESIAN_POINT('Ctrl Pts',(78.099126105575,79.5256823417411,199.610416665711));
#32121=CARTESIAN_POINT('Ctrl Pts',(78.5859406020177,80.0356346481401,199.668749999044));
#32122=CARTESIAN_POINT('Ctrl Pts',(78.3877161981791,80.7122045221895,199.727083332377));
#32123=CARTESIAN_POINT('Ctrl Pts',(78.1894917943405,81.388774396239,199.785416665711));
#32124=CARTESIAN_POINT('Ctrl Pts',(77.5044528940591,81.5553919638894,199.843749999044));
#32125=CARTESIAN_POINT('Ctrl Pts',(76.8194139937778,81.7220095315399,199.902083332377));
#32126=CARTESIAN_POINT('Ctrl Pts',(76.332599497335,81.2120572251409,199.960416665711));
#32127=CARTESIAN_POINT('Ctrl Pts',(75.8457850008923,80.702104918742,200.018749999044));
#32128=CARTESIAN_POINT('Ctrl Pts',(76.0440094047309,80.0255350446925,200.077083332377));
#32129=CARTESIAN_POINT('Ctrl Pts',(76.2422338085695,79.348965170643,200.135416665711));
#32130=CARTESIAN_POINT('Ctrl Pts',(76.9272727088508,79.1823476029926,200.193749999044));
#32131=CARTESIAN_POINT('Ctrl Pts',(77.6123116091322,79.0157300353421,200.252083332377));
#32132=CARTESIAN_POINT('Ctrl Pts',(78.099126105575,79.5256823417411,200.310416665711));
#32133=CARTESIAN_POINT('Ctrl Pts',(78.5859406020177,80.0356346481401,200.368749999044));
#32134=CARTESIAN_POINT('Ctrl Pts',(78.3877161981791,80.7122045221895,200.427083332377));
#32135=CARTESIAN_POINT('Ctrl Pts',(78.1894917943405,81.388774396239,200.485416665711));
#32136=CARTESIAN_POINT('Ctrl Pts',(77.5044528940591,81.5553919638894,200.543749999044));
#32137=CARTESIAN_POINT('Ctrl Pts',(76.8194139937778,81.7220095315399,200.602083332377));
#32138=CARTESIAN_POINT('Ctrl Pts',(76.332599497335,81.2120572251409,200.660416665711));
#32139=CARTESIAN_POINT('Ctrl Pts',(75.8457850008923,80.702104918742,200.718749999044));
#32140=CARTESIAN_POINT('Ctrl Pts',(76.0440094047309,80.0255350446925,200.777083332377));
#32141=CARTESIAN_POINT('Ctrl Pts',(76.2422338085695,79.348965170643,200.835416665711));
#32142=CARTESIAN_POINT('Ctrl Pts',(76.9272727088508,79.1823476029926,200.893749999044));
#32143=CARTESIAN_POINT('Ctrl Pts',(77.6123116091322,79.0157300353421,200.952083332377));
#32144=CARTESIAN_POINT('Ctrl Pts',(78.099126105575,79.5256823417411,201.010416665711));
#32145=CARTESIAN_POINT('Ctrl Pts',(78.5859406020177,80.0356346481401,201.068749999044));
#32146=CARTESIAN_POINT('Ctrl Pts',(78.3877161981791,80.7122045221895,201.127083332377));
#32147=CARTESIAN_POINT('Ctrl Pts',(78.1894917943405,81.388774396239,201.185416665711));
#32148=CARTESIAN_POINT('Ctrl Pts',(77.5044528940591,81.5553919638894,201.243749999044));
#32149=CARTESIAN_POINT('Ctrl Pts',(76.8194139937778,81.7220095315399,201.302083332377));
#32150=CARTESIAN_POINT('Ctrl Pts',(76.332599497335,81.2120572251409,201.360416665711));
#32151=CARTESIAN_POINT('Ctrl Pts',(75.8457850008923,80.702104918742,201.418749999044));
#32152=CARTESIAN_POINT('Ctrl Pts',(76.0440094047309,80.0255350446925,201.477083332377));
#32153=CARTESIAN_POINT('Ctrl Pts',(76.2422338085695,79.348965170643,201.535416665711));
#32154=CARTESIAN_POINT('Ctrl Pts',(76.9272727088508,79.1823476029926,201.593749999044));
#32155=CARTESIAN_POINT('Ctrl Pts',(77.6123116091322,79.0157300353421,201.652083332377));
#32156=CARTESIAN_POINT('Ctrl Pts',(78.099126105575,79.5256823417411,201.710416665711));
#32157=CARTESIAN_POINT('Ctrl Pts',(78.5859406020177,80.0356346481401,201.768749999044));
#32158=CARTESIAN_POINT('Ctrl Pts',(78.3877161981791,80.7122045221895,201.827083332377));
#32159=CARTESIAN_POINT('Ctrl Pts',(78.1894917943405,81.388774396239,201.885416665711));
#32160=CARTESIAN_POINT('Ctrl Pts',(77.5044528940591,81.5553919638894,201.943749999044));
#32161=CARTESIAN_POINT('Ctrl Pts',(76.8194139937778,81.7220095315399,202.002083332377));
#32162=CARTESIAN_POINT('Ctrl Pts',(76.332599497335,81.2120572251409,202.060416665711));
#32163=CARTESIAN_POINT('Ctrl Pts',(75.8457850008923,80.702104918742,202.118749999044));
#32164=CARTESIAN_POINT('Ctrl Pts',(76.0440094047309,80.0255350446925,202.177083332377));
#32165=CARTESIAN_POINT('Ctrl Pts',(76.2422338085695,79.348965170643,202.235416665711));
#32166=CARTESIAN_POINT('Ctrl Pts',(76.9272727088508,79.1823476029926,202.293749999044));
#32167=CARTESIAN_POINT('Ctrl Pts',(77.6123116091322,79.0157300353421,202.352083332377));
#32168=CARTESIAN_POINT('Ctrl Pts',(78.099126105575,79.5256823417411,202.410416665711));
#32169=CARTESIAN_POINT('Ctrl Pts',(78.5859406020177,80.0356346481401,202.468749999044));
#32170=CARTESIAN_POINT('Ctrl Pts',(78.3877161981791,80.7122045221895,202.527083332377));
#32171=CARTESIAN_POINT('Ctrl Pts',(78.1894917943405,81.388774396239,202.585416665711));
#32172=CARTESIAN_POINT('Ctrl Pts',(77.5044528940591,81.5553919638894,202.643749999044));
#32173=CARTESIAN_POINT('Ctrl Pts',(76.8194139937778,81.7220095315399,202.702083332377));
#32174=CARTESIAN_POINT('Ctrl Pts',(76.332599497335,81.2120572251409,202.760416665711));
#32175=CARTESIAN_POINT('Ctrl Pts',(75.8457850008923,80.7021049187419,202.818749999044));
#32176=CARTESIAN_POINT('Ctrl Pts',(76.0440094047309,80.0255350446925,202.877083332377));
#32177=CARTESIAN_POINT('Ctrl Pts',(76.2422338085695,79.348965170643,202.935416665711));
#32178=CARTESIAN_POINT('Ctrl Pts',(76.9272727088508,79.1823476029926,202.993749999044));
#32179=CARTESIAN_POINT('Ctrl Pts',(77.6123116091322,79.0157300353421,203.052083332377));
#32180=CARTESIAN_POINT('Ctrl Pts',(78.099126105575,79.5256823417411,203.110416665711));
#32181=CARTESIAN_POINT('Ctrl Pts',(78.5859406020177,80.0356346481401,203.168749999044));
#32182=CARTESIAN_POINT('Ctrl Pts',(78.3877161981791,80.7122045221895,203.227083332377));
#32183=CARTESIAN_POINT('Ctrl Pts',(78.1894917943405,81.388774396239,203.285416665711));
#32184=CARTESIAN_POINT('Ctrl Pts',(77.5044528940591,81.5553919638894,203.343749999044));
#32185=CARTESIAN_POINT('Ctrl Pts',(76.8194139937778,81.7220095315399,203.402083332378));
#32186=CARTESIAN_POINT('Ctrl Pts',(76.332599497335,81.2120572251409,203.460416665711));
#32187=CARTESIAN_POINT('Ctrl Pts',(75.8457850008923,80.7021049187419,203.518749999044));
#32188=CARTESIAN_POINT('Ctrl Pts',(76.0440094047309,80.0255350446925,203.577083332377));
#32189=CARTESIAN_POINT('Ctrl Pts',(76.2422338085695,79.348965170643,203.635416665711));
#32190=CARTESIAN_POINT('Ctrl Pts',(76.9272727088508,79.1823476029926,203.693749999044));
#32191=CARTESIAN_POINT('Ctrl Pts',(77.6123116091322,79.0157300353421,203.752083332377));
#32192=CARTESIAN_POINT('Ctrl Pts',(78.099126105575,79.5256823417411,203.810416665711));
#32193=CARTESIAN_POINT('Ctrl Pts',(78.5859406020177,80.03563464814,203.868749999044));
#32194=CARTESIAN_POINT('Ctrl Pts',(78.3877161981791,80.7122045221895,203.927083332377));
#32195=CARTESIAN_POINT('Ctrl Pts',(78.1894917943405,81.388774396239,203.985416665711));
#32196=CARTESIAN_POINT('Ctrl Pts',(77.5044528940591,81.5553919638894,204.043749999044));
#32197=CARTESIAN_POINT('Ctrl Pts',(76.8194139937778,81.7220095315399,204.102083332377));
#32198=CARTESIAN_POINT('Ctrl Pts',(76.332599497335,81.2120572251409,204.160416665711));
#32199=CARTESIAN_POINT('Ctrl Pts',(75.8457850008923,80.7021049187419,204.218749999044));
#32200=CARTESIAN_POINT('Ctrl Pts',(76.0440094047309,80.0255350446925,204.277083332377));
#32201=CARTESIAN_POINT('Ctrl Pts',(76.2422338085695,79.348965170643,204.335416665711));
#32202=CARTESIAN_POINT('Ctrl Pts',(76.9272727088508,79.1823476029926,204.393749999044));
#32203=CARTESIAN_POINT('Ctrl Pts',(77.6123116091322,79.0157300353421,204.452083332377));
#32204=CARTESIAN_POINT('Ctrl Pts',(78.099126105575,79.5256823417411,204.510416665711));
#32205=CARTESIAN_POINT('Ctrl Pts',(78.5859406020177,80.03563464814,204.568749999044));
#32206=CARTESIAN_POINT('Ctrl Pts',(78.3877161981791,80.7122045221895,204.627083332377));
#32207=CARTESIAN_POINT('Ctrl Pts',(78.1894917943405,81.388774396239,204.685416665711));
#32208=CARTESIAN_POINT('Ctrl Pts',(77.5044528940591,81.5553919638894,204.743749999044));
#32209=CARTESIAN_POINT('Ctrl Pts',(76.8194139937778,81.7220095315399,204.802083332378));
#32210=CARTESIAN_POINT('Ctrl Pts',(76.332599497335,81.2120572251409,204.860416665711));
#32211=CARTESIAN_POINT('Ctrl Pts',(75.8457850008923,80.7021049187419,204.918749999044));
#32212=CARTESIAN_POINT('Ctrl Pts',(76.0440094047309,80.0255350446925,204.977083332377));
#32213=CARTESIAN_POINT('Ctrl Pts',(76.2422338085695,79.348965170643,205.035416665711));
#32214=CARTESIAN_POINT('Ctrl Pts',(76.9272727088508,79.1823476029926,205.093749999044));
#32215=CARTESIAN_POINT('Ctrl Pts',(77.6123116091322,79.0157300353421,205.152083332377));
#32216=CARTESIAN_POINT('Ctrl Pts',(78.099126105575,79.5256823417411,205.210416665711));
#32217=CARTESIAN_POINT('Ctrl Pts',(78.5859406020177,80.03563464814,205.268749999044));
#32218=CARTESIAN_POINT('Ctrl Pts',(78.3877161981791,80.7122045221895,205.327083332377));
#32219=CARTESIAN_POINT('Ctrl Pts',(78.1894917943405,81.388774396239,205.385416665711));
#32220=CARTESIAN_POINT('Ctrl Pts',(77.5044528940591,81.5553919638894,205.443749999044));
#32221=CARTESIAN_POINT('Ctrl Pts',(76.8194139937778,81.7220095315399,205.502083332377));
#32222=CARTESIAN_POINT('Ctrl Pts',(76.332599497335,81.2120572251409,205.560416665711));
#32223=CARTESIAN_POINT('Ctrl Pts',(75.8457850008923,80.7021049187419,205.618749999044));
#32224=CARTESIAN_POINT('Ctrl Pts',(76.0440094047309,80.0255350446925,205.677083332377));
#32225=CARTESIAN_POINT('Ctrl Pts',(76.2422338085695,79.348965170643,205.735416665711));
#32226=CARTESIAN_POINT('Ctrl Pts',(76.9272727088508,79.1823476029926,205.793749999044));
#32227=CARTESIAN_POINT('Ctrl Pts',(77.6123116091322,79.0157300353421,205.852083332377));
#32228=CARTESIAN_POINT('Ctrl Pts',(78.099126105575,79.5256823417411,205.910416665711));
#32229=CARTESIAN_POINT('Ctrl Pts',(78.5859406020177,80.03563464814,205.968749999044));
#32230=CARTESIAN_POINT('Ctrl Pts',(78.3877161981791,80.7122045221895,206.027083332377));
#32231=CARTESIAN_POINT('Ctrl Pts',(78.1894917943405,81.3887743962389,206.085416665711));
#32232=CARTESIAN_POINT('Ctrl Pts',(77.5044528940591,81.5553919638894,206.143749999044));
#32233=CARTESIAN_POINT('Ctrl Pts',(76.8194139937778,81.7220095315399,206.202083332377));
#32234=CARTESIAN_POINT('Ctrl Pts',(76.332599497335,81.2120572251409,206.260416665711));
#32235=CARTESIAN_POINT('Ctrl Pts',(75.8457850008923,80.7021049187419,206.318749999044));
#32236=CARTESIAN_POINT('Ctrl Pts',(76.0440094047309,80.0255350446925,206.377083332377));
#32237=CARTESIAN_POINT('Ctrl Pts',(76.2422338085695,79.348965170643,206.435416665711));
#32238=CARTESIAN_POINT('Ctrl Pts',(76.9272727088508,79.1823476029926,206.493749999044));
#32239=CARTESIAN_POINT('Ctrl Pts',(77.6123116091322,79.0157300353421,206.552083332377));
#32240=CARTESIAN_POINT('Ctrl Pts',(78.099126105575,79.5256823417411,206.610416665711));
#32241=CARTESIAN_POINT('Ctrl Pts',(78.5859406020177,80.03563464814,206.668749999044));
#32242=CARTESIAN_POINT('Ctrl Pts',(78.3877161981791,80.7122045221895,206.727083332377));
#32243=CARTESIAN_POINT('Ctrl Pts',(78.1894917943405,81.3887743962389,206.785416665711));
#32244=CARTESIAN_POINT('Ctrl Pts',(77.5044528940591,81.5553919638894,206.843749999044));
#32245=CARTESIAN_POINT('Ctrl Pts',(76.8194139937778,81.7220095315399,206.902083332377));
#32246=CARTESIAN_POINT('Ctrl Pts',(76.332599497335,81.2120572251409,206.960416665711));
#32247=CARTESIAN_POINT('Ctrl Pts',(75.8457850008923,80.7021049187419,207.018749999044));
#32248=CARTESIAN_POINT('Ctrl Pts',(76.0440094047309,80.0255350446925,207.077083332377));
#32249=CARTESIAN_POINT('Ctrl Pts',(76.2422338085695,79.348965170643,207.135416665711));
#32250=CARTESIAN_POINT('Ctrl Pts',(76.9272727088508,79.1823476029926,207.193749999044));
#32251=CARTESIAN_POINT('Ctrl Pts',(77.6123116091322,79.0157300353421,207.252083332377));
#32252=CARTESIAN_POINT('Ctrl Pts',(78.099126105575,79.5256823417411,207.310416665711));
#32253=CARTESIAN_POINT('Ctrl Pts',(78.5859406020177,80.03563464814,207.368749999044));
#32254=CARTESIAN_POINT('Ctrl Pts',(78.3877161981791,80.7122045221895,207.427083332377));
#32255=CARTESIAN_POINT('Ctrl Pts',(78.1894917943405,81.3887743962389,207.485416665711));
#32256=CARTESIAN_POINT('Ctrl Pts',(77.5044528940591,81.5553919638894,207.543749999044));
#32257=CARTESIAN_POINT('Ctrl Pts',(76.8194139937778,81.7220095315399,207.602083332378));
#32258=CARTESIAN_POINT('Ctrl Pts',(76.332599497335,81.2120572251409,207.660416665711));
#32259=CARTESIAN_POINT('Ctrl Pts',(75.8457850008923,80.7021049187419,207.718749999044));
#32260=CARTESIAN_POINT('Ctrl Pts',(76.0440094047309,80.0255350446925,207.777083332377));
#32261=CARTESIAN_POINT('Ctrl Pts',(76.2422338085695,79.348965170643,207.835416665711));
#32262=CARTESIAN_POINT('Ctrl Pts',(76.9272727088508,79.1823476029926,207.893749999044));
#32263=CARTESIAN_POINT('Ctrl Pts',(77.6123116091322,79.0157300353421,207.952083332377));
#32264=CARTESIAN_POINT('Ctrl Pts',(78.0991261055749,79.5256823417411,208.010416665711));
#32265=CARTESIAN_POINT('Ctrl Pts',(78.5859406020177,80.03563464814,208.068749999044));
#32266=CARTESIAN_POINT('Ctrl Pts',(78.3877161981791,80.7122045221895,208.127083332377));
#32267=CARTESIAN_POINT('Ctrl Pts',(78.1894917943405,81.3887743962389,208.185416665711));
#32268=CARTESIAN_POINT('Ctrl Pts',(77.5044528940591,81.5553919638894,208.243749999044));
#32269=CARTESIAN_POINT('Ctrl Pts',(76.8194139937778,81.7220095315399,208.302083332377));
#32270=CARTESIAN_POINT('Ctrl Pts',(76.332599497335,81.2120572251409,208.360416665711));
#32271=CARTESIAN_POINT('Ctrl Pts',(75.8457850008923,80.7021049187419,208.418749999044));
#32272=CARTESIAN_POINT('Ctrl Pts',(76.0440094047309,80.0255350446925,208.477083332377));
#32273=CARTESIAN_POINT('Ctrl Pts',(76.2422338085695,79.348965170643,208.535416665711));
#32274=CARTESIAN_POINT('Ctrl Pts',(76.9272727088508,79.1823476029926,208.593749999044));
#32275=CARTESIAN_POINT('Ctrl Pts',(77.6123116091322,79.0157300353421,208.652083332377));
#32276=CARTESIAN_POINT('Ctrl Pts',(78.0991261055749,79.5256823417411,208.710416665711));
#32277=CARTESIAN_POINT('Ctrl Pts',(78.5859406020177,80.03563464814,208.768749999044));
#32278=CARTESIAN_POINT('Ctrl Pts',(78.3877161981791,80.7122045221895,208.827083332377));
#32279=CARTESIAN_POINT('Ctrl Pts',(78.1894917943405,81.3887743962389,208.885416665711));
#32280=CARTESIAN_POINT('Ctrl Pts',(77.5044528940591,81.5553919638894,208.943749999044));
#32281=CARTESIAN_POINT('Ctrl Pts',(76.8194139937778,81.7220095315399,209.002083332377));
#32282=CARTESIAN_POINT('Ctrl Pts',(76.332599497335,81.2120572251409,209.060416665711));
#32283=CARTESIAN_POINT('Ctrl Pts',(75.8457850008923,80.7021049187419,209.118749999044));
#32284=CARTESIAN_POINT('Ctrl Pts',(76.0440094047309,80.0255350446925,209.177083332377));
#32285=CARTESIAN_POINT('Ctrl Pts',(76.2422338085695,79.348965170643,209.235416665711));
#32286=CARTESIAN_POINT('Ctrl Pts',(76.9272727088508,79.1823476029926,209.293749999044));
#32287=CARTESIAN_POINT('Ctrl Pts',(77.6123116091322,79.0157300353421,209.352083332377));
#32288=CARTESIAN_POINT('Ctrl Pts',(78.0991261055749,79.5256823417411,209.410416665711));
#32289=CARTESIAN_POINT('Ctrl Pts',(78.5859406020177,80.03563464814,209.468749999044));
#32290=CARTESIAN_POINT('Ctrl Pts',(78.3877161981791,80.7122045221895,209.527083332377));
#32291=CARTESIAN_POINT('Ctrl Pts',(78.1894917943405,81.3887743962389,209.585416665711));
#32292=CARTESIAN_POINT('Ctrl Pts',(77.5044528940591,81.5553919638894,209.643749999044));
#32293=CARTESIAN_POINT('Ctrl Pts',(76.8194139937778,81.7220095315399,209.702083332377));
#32294=CARTESIAN_POINT('Ctrl Pts',(76.332599497335,81.2120572251409,209.760416665711));
#32295=CARTESIAN_POINT('Ctrl Pts',(75.8457850008923,80.7021049187419,209.818749999044));
#32296=CARTESIAN_POINT('Ctrl Pts',(76.0440094047309,80.0255350446925,209.877083332377));
#32297=CARTESIAN_POINT('Ctrl Pts',(76.2422338085695,79.348965170643,209.935416665711));
#32298=CARTESIAN_POINT('Ctrl Pts',(76.9272727088508,79.1823476029926,209.993749999044));
#32299=CARTESIAN_POINT('Ctrl Pts',(77.6123116091322,79.0157300353421,210.052083332377));
#32300=CARTESIAN_POINT('Ctrl Pts',(78.0991261055749,79.5256823417411,210.110416665711));
#32301=CARTESIAN_POINT('Ctrl Pts',(78.5859406020177,80.03563464814,210.168749999044));
#32302=CARTESIAN_POINT('Ctrl Pts',(78.3877161981791,80.7122045221895,210.227083332377));
#32303=CARTESIAN_POINT('Ctrl Pts',(78.1894917943405,81.3887743962389,210.285416665711));
#32304=CARTESIAN_POINT('Ctrl Pts',(77.5044528940591,81.5553919638894,210.343749999044));
#32305=CARTESIAN_POINT('Ctrl Pts',(76.8194139937778,81.7220095315399,210.402083332377));
#32306=CARTESIAN_POINT('Ctrl Pts',(76.332599497335,81.2120572251409,210.460416665711));
#32307=CARTESIAN_POINT('Ctrl Pts',(75.8457850008923,80.7021049187419,210.518749999044));
#32308=CARTESIAN_POINT('Ctrl Pts',(76.0440094047309,80.0255350446925,210.577083332377));
#32309=CARTESIAN_POINT('Ctrl Pts',(76.2422338085695,79.348965170643,210.635416665711));
#32310=CARTESIAN_POINT('Ctrl Pts',(76.9272727088508,79.1823476029926,210.693749999044));
#32311=CARTESIAN_POINT('Ctrl Pts',(77.6123116091322,79.0157300353421,210.752083332377));
#32312=CARTESIAN_POINT('Ctrl Pts',(78.0991261055749,79.5256823417411,210.810416665711));
#32313=CARTESIAN_POINT('Ctrl Pts',(78.5859406020177,80.03563464814,210.868749999044));
#32314=CARTESIAN_POINT('Ctrl Pts',(78.3877161981791,80.7122045221895,210.927083332377));
#32315=CARTESIAN_POINT('Ctrl Pts',(78.1894917943405,81.3887743962389,210.985416665711));
#32316=CARTESIAN_POINT('Ctrl Pts',(77.5044528940591,81.5553919638894,211.043749999044));
#32317=CARTESIAN_POINT('Ctrl Pts',(76.8194139937778,81.7220095315399,211.102083332377));
#32318=CARTESIAN_POINT('Ctrl Pts',(76.332599497335,81.2120572251409,211.160416665711));
#32319=CARTESIAN_POINT('Ctrl Pts',(75.8457850008923,80.7021049187419,211.218749999044));
#32320=CARTESIAN_POINT('Ctrl Pts',(76.0440094047309,80.0255350446925,211.277083332377));
#32321=CARTESIAN_POINT('Ctrl Pts',(76.2422338085695,79.348965170643,211.335416665711));
#32322=CARTESIAN_POINT('Ctrl Pts',(76.9272727088508,79.1823476029925,211.393749999044));
#32323=CARTESIAN_POINT('Ctrl Pts',(77.6123116091322,79.0157300353421,211.452083332377));
#32324=CARTESIAN_POINT('Ctrl Pts',(78.0991261055749,79.525682341741,211.510416665711));
#32325=CARTESIAN_POINT('Ctrl Pts',(78.5859406020177,80.03563464814,211.568749999044));
#32326=CARTESIAN_POINT('Ctrl Pts',(78.3877161981791,80.7122045221895,211.627083332377));
#32327=CARTESIAN_POINT('Ctrl Pts',(78.1894917943405,81.3887743962389,211.685416665711));
#32328=CARTESIAN_POINT('Ctrl Pts',(77.5044528940591,81.5553919638894,211.743749999044));
#32329=CARTESIAN_POINT('Ctrl Pts',(76.8194139937778,81.7220095315399,211.802083332377));
#32330=CARTESIAN_POINT('Ctrl Pts',(76.332599497335,81.2120572251409,211.860416665711));
#32331=CARTESIAN_POINT('Ctrl Pts',(75.8457850008923,80.7021049187419,211.918749999044));
#32332=CARTESIAN_POINT('Ctrl Pts',(76.0440094047309,80.0255350446925,211.977083332377));
#32333=CARTESIAN_POINT('Ctrl Pts',(76.2422338085695,79.348965170643,212.035416665711));
#32334=CARTESIAN_POINT('Ctrl Pts',(76.9272727088508,79.1823476029925,212.093749999044));
#32335=CARTESIAN_POINT('',(76.882500972401,78.9982710885302,198.203124998566));
#32336=CARTESIAN_POINT('Ctrl Pts',(76.8377292359513,78.8141945740678,210.212499998088));
#32337=CARTESIAN_POINT('Ctrl Pts',(76.8592837264637,78.8089520151713,210.213900796078));
#32338=CARTESIAN_POINT('Ctrl Pts',(76.880961717515,78.8041541885631,210.215319353774));
#32339=CARTESIAN_POINT('Ctrl Pts',(77.1109710529602,78.7582549040848,210.230473284417));
#32340=CARTESIAN_POINT('Ctrl Pts',(77.3253356333712,78.7585744965251,210.245480033072));
#32341=CARTESIAN_POINT('Ctrl Pts',(77.737156513034,78.8419446966982,210.276006491287));
#32342=CARTESIAN_POINT('Ctrl Pts',(77.9310168188607,78.9225572032128,210.291224585572));
#32343=CARTESIAN_POINT('Ctrl Pts',(78.2736586329449,79.1512256470014,210.319889078168));
#32344=CARTESIAN_POINT('Ctrl Pts',(78.4200352333683,79.2957652859252,210.332220462871));
#32345=CARTESIAN_POINT('Ctrl Pts',(78.6562261084613,79.6401624127909,210.360691567112));
#32346=CARTESIAN_POINT('Ctrl Pts',(78.7405435897384,79.8387937024458,210.376217822852));
#32347=CARTESIAN_POINT('Ctrl Pts',(78.8245801400631,80.2494216513298,210.406759430467));
#32348=CARTESIAN_POINT('Ctrl Pts',(78.8266170207136,80.4568794737522,210.42149314287));
#32349=CARTESIAN_POINT('Ctrl Pts',(78.7514066787451,80.8646581040814,210.449088627304));
#32350=CARTESIAN_POINT('Ctrl Pts',(78.6735850260427,81.0608017958442,210.462121129468));
#32351=CARTESIAN_POINT('Ctrl Pts',(78.4457682921329,81.4137915170909,210.49190959644));
#32352=CARTESIAN_POINT('Ctrl Pts',(78.2973923216281,81.5667079258093,210.507434575797));
#32353=CARTESIAN_POINT('Ctrl Pts',(77.9562152832965,81.8017739525743,210.537264556535));
#32354=CARTESIAN_POINT('Ctrl Pts',(77.7684344389729,81.8840950144953,210.551102454384));
#32355=CARTESIAN_POINT('Ctrl Pts',(77.3633866713352,81.9761357117601,210.577558753721));
#32356=CARTESIAN_POINT('Ctrl Pts',(77.1491313794517,81.9814958308773,210.592441411551));
#32357=CARTESIAN_POINT('Ctrl Pts',(76.7347602170159,81.9090030673567,210.622923321041));
#32358=CARTESIAN_POINT('Ctrl Pts',(76.538357199793,81.8332707638251,210.638219289857));
#32359=CARTESIAN_POINT('Ctrl Pts',(76.1900091522267,81.6134527075351,210.667101629704));
#32360=CARTESIAN_POINT('Ctrl Pts',(76.0403356127154,81.4731739150612,210.679516301547));
#32361=CARTESIAN_POINT('Ctrl Pts',(75.7950649908508,81.1351846320785,210.707689871198));
#32362=CARTESIAN_POINT('Ctrl Pts',(75.7053556877558,80.9382903200132,210.723185975568));
#32363=CARTESIAN_POINT('Ctrl Pts',(75.610609672748,80.5289041559014,210.753824153838));
#32364=CARTESIAN_POINT('Ctrl Pts',(75.6033512671848,80.3210446090024,210.768676309564));
#32365=CARTESIAN_POINT('Ctrl Pts',(75.6683527121138,79.9124473561696,210.796505720633));
#32366=CARTESIAN_POINT('Ctrl Pts',(75.7405496446513,79.7157440358032,210.809239465238));
#32367=CARTESIAN_POINT('Ctrl Pts',(75.958191918574,79.3574194143084,210.838759914931));
#32368=CARTESIAN_POINT('Ctrl Pts',(76.1028124562074,79.2001630186463,210.854305339291));
#32369=CARTESIAN_POINT('Ctrl Pts',(76.4383986735495,78.9557132669801,210.884312911503));
#32370=CARTESIAN_POINT('Ctrl Pts',(76.6244149216965,78.8683037668432,210.898524896631));
#32371=CARTESIAN_POINT('Ctrl Pts',(76.8271568598205,78.8167946101776,210.911811473997));
#32372=CARTESIAN_POINT('Ctrl Pts',(76.8324403040916,78.8154809666531,210.912156277363));
#32373=CARTESIAN_POINT('Ctrl Pts',(76.8377292359511,78.8141945740678,210.912499998088));
#32374=CARTESIAN_POINT('Ctrl Pts',(76.6545412773313,78.870564692161,211.6));
#32375=CARTESIAN_POINT('Ctrl Pts',(76.7444440687127,78.8368837201247,211.60643751776));
#32376=CARTESIAN_POINT('Ctrl Pts',(76.8377292359511,78.8141945740679,211.612499998088));
#32377=CARTESIAN_POINT('Ctrl Pts',(77.7353213865851,78.5958790582345,211.670833331422));
#32378=CARTESIAN_POINT('Ctrl Pts',(78.3731842446541,79.2640589050045,211.729166664755));
#32379=CARTESIAN_POINT('Ctrl Pts',(79.011047102723,79.9322387517744,211.787499998088));
#32380=CARTESIAN_POINT('Ctrl Pts',(78.7513178101579,80.8187341143776,211.845833331422));
#32381=CARTESIAN_POINT('Ctrl Pts',(78.4915885175929,81.7052294769808,211.904166664755));
#32382=CARTESIAN_POINT('Ctrl Pts',(77.5939963669588,81.9235449928141,211.962499998088));
#32383=CARTESIAN_POINT('',(76.882500972401,78.9982710885302,212.203124998566));
#32384=CARTESIAN_POINT('Ctrl Pts',(77.5044528940591,81.5553919638894,198.443749999044));
#32385=CARTESIAN_POINT('Ctrl Pts',(76.8194139937778,81.7220095315399,198.502083332377));
#32386=CARTESIAN_POINT('Ctrl Pts',(76.332599497335,81.2120572251409,198.560416665711));
#32387=CARTESIAN_POINT('Ctrl Pts',(75.8457850008923,80.702104918742,198.618749999044));
#32388=CARTESIAN_POINT('Ctrl Pts',(76.0440094047309,80.0255350446925,198.677083332377));
#32389=CARTESIAN_POINT('Ctrl Pts',(76.2422338085695,79.3489651706431,198.735416665711));
#32390=CARTESIAN_POINT('Ctrl Pts',(76.9272727088509,79.1823476029926,198.793749999044));
#32391=CARTESIAN_POINT('Ctrl Pts',(77.6123116091322,79.0157300353421,198.852083332378));
#32392=CARTESIAN_POINT('Ctrl Pts',(78.099126105575,79.5256823417411,198.910416665711));
#32393=CARTESIAN_POINT('Ctrl Pts',(78.5859406020177,80.0356346481401,198.968749999044));
#32394=CARTESIAN_POINT('Ctrl Pts',(78.3877161981791,80.7122045221895,199.027083332377));
#32395=CARTESIAN_POINT('Ctrl Pts',(78.1894917943405,81.388774396239,199.085416665711));
#32396=CARTESIAN_POINT('Ctrl Pts',(77.5044528940591,81.5553919638894,199.143749999044));
#32397=CARTESIAN_POINT('Origin',(77.2158628014549,80.3688697834408,198.006249999044));
#32398=CARTESIAN_POINT('Ctrl Pts',(77.5044528940591,81.5553919638894,198.268749999044));
#32399=CARTESIAN_POINT('Ctrl Pts',(76.8194139937778,81.7220095315399,198.327083332377));
#32400=CARTESIAN_POINT('Ctrl Pts',(76.332599497335,81.2120572251409,198.385416665711));
#32401=CARTESIAN_POINT('Ctrl Pts',(75.8457850008923,80.702104918742,198.443749999044));
#32402=CARTESIAN_POINT('Ctrl Pts',(76.0440094047309,80.0255350446925,198.502083332377));
#32403=CARTESIAN_POINT('Ctrl Pts',(76.2422338085695,79.3489651706431,198.560416665711));
#32404=CARTESIAN_POINT('Ctrl Pts',(76.9272727088509,79.1823476029926,198.618749999044));
#32405=CARTESIAN_POINT('Ctrl Pts',(77.6123116091322,79.0157300353421,198.677083332377));
#32406=CARTESIAN_POINT('Ctrl Pts',(78.099126105575,79.5256823417411,198.735416665711));
#32407=CARTESIAN_POINT('Ctrl Pts',(78.5859406020177,80.0356346481401,198.793749999044));
#32408=CARTESIAN_POINT('Ctrl Pts',(78.3877161981791,80.7122045221895,198.852083332377));
#32409=CARTESIAN_POINT('Ctrl Pts',(78.1894917943405,81.388774396239,198.910416665711));
#32410=CARTESIAN_POINT('Ctrl Pts',(77.5044528940591,81.5553919638894,198.968749999044));
#32411=CARTESIAN_POINT('Ctrl Pts',(76.9272727088509,79.1823476029926,197.918749999044));
#32412=CARTESIAN_POINT('Ctrl Pts',(77.6123116091322,79.0157300353421,197.977083332377));
#32413=CARTESIAN_POINT('Ctrl Pts',(78.099126105575,79.5256823417411,198.035416665711));
#32414=CARTESIAN_POINT('Ctrl Pts',(78.5859406020177,80.0356346481401,198.093749999044));
#32415=CARTESIAN_POINT('Ctrl Pts',(78.3877161981791,80.7122045221895,198.152083332377));
#32416=CARTESIAN_POINT('Ctrl Pts',(78.1894917943405,81.388774396239,198.210416665711));
#32417=CARTESIAN_POINT('Ctrl Pts',(77.5044528940591,81.5553919638894,198.268749999044));
#32418=CARTESIAN_POINT('Ctrl Pts',(76.8194139937778,81.7220095315399,198.327083332377));
#32419=CARTESIAN_POINT('Ctrl Pts',(76.332599497335,81.2120572251409,198.385416665711));
#32420=CARTESIAN_POINT('Ctrl Pts',(75.8457850008923,80.702104918742,198.443749999044));
#32421=CARTESIAN_POINT('Ctrl Pts',(76.0440094047309,80.0255350446925,198.502083332377));
#32422=CARTESIAN_POINT('Ctrl Pts',(76.2422338085695,79.348965170643,198.560416665711));
#32423=CARTESIAN_POINT('Ctrl Pts',(76.9272727088509,79.1823476029926,198.618749999044));
#32424=CARTESIAN_POINT('Ctrl Pts',(77.6123116091322,79.0157300353421,198.677083332377));
#32425=CARTESIAN_POINT('Ctrl Pts',(78.099126105575,79.5256823417411,198.735416665711));
#32426=CARTESIAN_POINT('Ctrl Pts',(78.5859406020177,80.0356346481401,198.793749999044));
#32427=CARTESIAN_POINT('Ctrl Pts',(78.3877161981791,80.7122045221895,198.852083332377));
#32428=CARTESIAN_POINT('Ctrl Pts',(78.1894917943405,81.388774396239,198.910416665711));
#32429=CARTESIAN_POINT('Ctrl Pts',(77.5044528940591,81.5553919638894,198.968749999044));
#32430=CARTESIAN_POINT('Ctrl Pts',(76.8194139937778,81.7220095315399,199.027083332377));
#32431=CARTESIAN_POINT('Ctrl Pts',(76.332599497335,81.2120572251409,199.085416665711));
#32432=CARTESIAN_POINT('Ctrl Pts',(75.8457850008923,80.702104918742,199.143749999044));
#32433=CARTESIAN_POINT('Ctrl Pts',(76.0440094047309,80.0255350446925,199.202083332377));
#32434=CARTESIAN_POINT('Ctrl Pts',(76.2422338085695,79.348965170643,199.260416665711));
#32435=CARTESIAN_POINT('Ctrl Pts',(76.9272727088509,79.1823476029926,199.318749999044));
#32436=CARTESIAN_POINT('Ctrl Pts',(77.6123116091322,79.0157300353421,199.377083332377));
#32437=CARTESIAN_POINT('Ctrl Pts',(78.099126105575,79.5256823417411,199.435416665711));
#32438=CARTESIAN_POINT('Ctrl Pts',(78.5859406020177,80.0356346481401,199.493749999044));
#32439=CARTESIAN_POINT('Ctrl Pts',(78.3877161981791,80.7122045221895,199.552083332377));
#32440=CARTESIAN_POINT('Ctrl Pts',(78.1894917943405,81.388774396239,199.610416665711));
#32441=CARTESIAN_POINT('Ctrl Pts',(77.5044528940591,81.5553919638894,199.668749999044));
#32442=CARTESIAN_POINT('Ctrl Pts',(76.8194139937778,81.7220095315399,199.727083332377));
#32443=CARTESIAN_POINT('Ctrl Pts',(76.332599497335,81.2120572251409,199.785416665711));
#32444=CARTESIAN_POINT('Ctrl Pts',(75.8457850008923,80.702104918742,199.843749999044));
#32445=CARTESIAN_POINT('Ctrl Pts',(76.0440094047309,80.0255350446925,199.902083332377));
#32446=CARTESIAN_POINT('Ctrl Pts',(76.2422338085695,79.348965170643,199.960416665711));
#32447=CARTESIAN_POINT('Ctrl Pts',(76.9272727088508,79.1823476029926,200.018749999044));
#32448=CARTESIAN_POINT('Ctrl Pts',(77.6123116091322,79.0157300353421,200.077083332377));
#32449=CARTESIAN_POINT('Ctrl Pts',(78.099126105575,79.5256823417411,200.135416665711));
#32450=CARTESIAN_POINT('Ctrl Pts',(78.5859406020177,80.0356346481401,200.193749999044));
#32451=CARTESIAN_POINT('Ctrl Pts',(78.3877161981791,80.7122045221895,200.252083332377));
#32452=CARTESIAN_POINT('Ctrl Pts',(78.1894917943405,81.388774396239,200.310416665711));
#32453=CARTESIAN_POINT('Ctrl Pts',(77.5044528940591,81.5553919638894,200.368749999044));
#32454=CARTESIAN_POINT('Ctrl Pts',(76.8194139937778,81.7220095315399,200.427083332377));
#32455=CARTESIAN_POINT('Ctrl Pts',(76.332599497335,81.2120572251409,200.485416665711));
#32456=CARTESIAN_POINT('Ctrl Pts',(75.8457850008923,80.702104918742,200.543749999044));
#32457=CARTESIAN_POINT('Ctrl Pts',(76.0440094047309,80.0255350446925,200.602083332377));
#32458=CARTESIAN_POINT('Ctrl Pts',(76.2422338085695,79.348965170643,200.660416665711));
#32459=CARTESIAN_POINT('Ctrl Pts',(76.9272727088508,79.1823476029926,200.718749999044));
#32460=CARTESIAN_POINT('Ctrl Pts',(77.6123116091322,79.0157300353421,200.777083332377));
#32461=CARTESIAN_POINT('Ctrl Pts',(78.099126105575,79.5256823417411,200.835416665711));
#32462=CARTESIAN_POINT('Ctrl Pts',(78.5859406020177,80.0356346481401,200.893749999044));
#32463=CARTESIAN_POINT('Ctrl Pts',(78.3877161981791,80.7122045221895,200.952083332377));
#32464=CARTESIAN_POINT('Ctrl Pts',(78.1894917943405,81.388774396239,201.010416665711));
#32465=CARTESIAN_POINT('Ctrl Pts',(77.5044528940591,81.5553919638894,201.068749999044));
#32466=CARTESIAN_POINT('Ctrl Pts',(76.8194139937778,81.7220095315399,201.127083332377));
#32467=CARTESIAN_POINT('Ctrl Pts',(76.332599497335,81.2120572251409,201.185416665711));
#32468=CARTESIAN_POINT('Ctrl Pts',(75.8457850008923,80.702104918742,201.243749999044));
#32469=CARTESIAN_POINT('Ctrl Pts',(76.0440094047309,80.0255350446925,201.302083332377));
#32470=CARTESIAN_POINT('Ctrl Pts',(76.2422338085695,79.348965170643,201.360416665711));
#32471=CARTESIAN_POINT('Ctrl Pts',(76.9272727088508,79.1823476029926,201.418749999044));
#32472=CARTESIAN_POINT('Ctrl Pts',(77.6123116091322,79.0157300353421,201.477083332377));
#32473=CARTESIAN_POINT('Ctrl Pts',(78.099126105575,79.5256823417411,201.535416665711));
#32474=CARTESIAN_POINT('Ctrl Pts',(78.5859406020177,80.0356346481401,201.593749999044));
#32475=CARTESIAN_POINT('Ctrl Pts',(78.3877161981791,80.7122045221895,201.652083332377));
#32476=CARTESIAN_POINT('Ctrl Pts',(78.1894917943405,81.388774396239,201.710416665711));
#32477=CARTESIAN_POINT('Ctrl Pts',(77.5044528940591,81.5553919638894,201.768749999044));
#32478=CARTESIAN_POINT('Ctrl Pts',(76.8194139937778,81.7220095315399,201.827083332377));
#32479=CARTESIAN_POINT('Ctrl Pts',(76.332599497335,81.2120572251409,201.885416665711));
#32480=CARTESIAN_POINT('Ctrl Pts',(75.8457850008923,80.702104918742,201.943749999044));
#32481=CARTESIAN_POINT('Ctrl Pts',(76.0440094047309,80.0255350446925,202.002083332377));
#32482=CARTESIAN_POINT('Ctrl Pts',(76.2422338085695,79.348965170643,202.060416665711));
#32483=CARTESIAN_POINT('Ctrl Pts',(76.9272727088508,79.1823476029926,202.118749999044));
#32484=CARTESIAN_POINT('Ctrl Pts',(77.6123116091322,79.0157300353421,202.177083332377));
#32485=CARTESIAN_POINT('Ctrl Pts',(78.099126105575,79.5256823417411,202.235416665711));
#32486=CARTESIAN_POINT('Ctrl Pts',(78.5859406020177,80.0356346481401,202.293749999044));
#32487=CARTESIAN_POINT('Ctrl Pts',(78.3877161981791,80.7122045221895,202.352083332377));
#32488=CARTESIAN_POINT('Ctrl Pts',(78.1894917943405,81.388774396239,202.410416665711));
#32489=CARTESIAN_POINT('Ctrl Pts',(77.5044528940591,81.5553919638894,202.468749999044));
#32490=CARTESIAN_POINT('Ctrl Pts',(76.8194139937778,81.7220095315399,202.527083332377));
#32491=CARTESIAN_POINT('Ctrl Pts',(76.332599497335,81.2120572251409,202.585416665711));
#32492=CARTESIAN_POINT('Ctrl Pts',(75.8457850008923,80.702104918742,202.643749999044));
#32493=CARTESIAN_POINT('Ctrl Pts',(76.0440094047309,80.0255350446925,202.702083332377));
#32494=CARTESIAN_POINT('Ctrl Pts',(76.2422338085695,79.348965170643,202.760416665711));
#32495=CARTESIAN_POINT('Ctrl Pts',(76.9272727088508,79.1823476029926,202.818749999044));
#32496=CARTESIAN_POINT('Ctrl Pts',(77.6123116091322,79.0157300353421,202.877083332377));
#32497=CARTESIAN_POINT('Ctrl Pts',(78.099126105575,79.5256823417411,202.935416665711));
#32498=CARTESIAN_POINT('Ctrl Pts',(78.5859406020177,80.0356346481401,202.993749999044));
#32499=CARTESIAN_POINT('Ctrl Pts',(78.3877161981791,80.7122045221895,203.052083332377));
#32500=CARTESIAN_POINT('Ctrl Pts',(78.1894917943405,81.388774396239,203.110416665711));
#32501=CARTESIAN_POINT('Ctrl Pts',(77.5044528940591,81.5553919638894,203.168749999044));
#32502=CARTESIAN_POINT('Ctrl Pts',(76.8194139937778,81.7220095315399,203.227083332378));
#32503=CARTESIAN_POINT('Ctrl Pts',(76.332599497335,81.2120572251409,203.285416665711));
#32504=CARTESIAN_POINT('Ctrl Pts',(75.8457850008923,80.7021049187419,203.343749999044));
#32505=CARTESIAN_POINT('Ctrl Pts',(76.0440094047309,80.0255350446925,203.402083332377));
#32506=CARTESIAN_POINT('Ctrl Pts',(76.2422338085695,79.348965170643,203.460416665711));
#32507=CARTESIAN_POINT('Ctrl Pts',(76.9272727088508,79.1823476029926,203.518749999044));
#32508=CARTESIAN_POINT('Ctrl Pts',(77.6123116091322,79.0157300353421,203.577083332377));
#32509=CARTESIAN_POINT('Ctrl Pts',(78.099126105575,79.5256823417411,203.635416665711));
#32510=CARTESIAN_POINT('Ctrl Pts',(78.5859406020177,80.0356346481401,203.693749999044));
#32511=CARTESIAN_POINT('Ctrl Pts',(78.3877161981791,80.7122045221895,203.752083332377));
#32512=CARTESIAN_POINT('Ctrl Pts',(78.1894917943405,81.388774396239,203.810416665711));
#32513=CARTESIAN_POINT('Ctrl Pts',(77.5044528940591,81.5553919638894,203.868749999044));
#32514=CARTESIAN_POINT('Ctrl Pts',(76.8194139937778,81.7220095315399,203.927083332377));
#32515=CARTESIAN_POINT('Ctrl Pts',(76.332599497335,81.2120572251409,203.985416665711));
#32516=CARTESIAN_POINT('Ctrl Pts',(75.8457850008923,80.7021049187419,204.043749999044));
#32517=CARTESIAN_POINT('Ctrl Pts',(76.0440094047309,80.0255350446925,204.102083332377));
#32518=CARTESIAN_POINT('Ctrl Pts',(76.2422338085695,79.348965170643,204.160416665711));
#32519=CARTESIAN_POINT('Ctrl Pts',(76.9272727088508,79.1823476029926,204.218749999044));
#32520=CARTESIAN_POINT('Ctrl Pts',(77.6123116091322,79.0157300353421,204.277083332377));
#32521=CARTESIAN_POINT('Ctrl Pts',(78.099126105575,79.5256823417411,204.335416665711));
#32522=CARTESIAN_POINT('Ctrl Pts',(78.5859406020177,80.03563464814,204.393749999044));
#32523=CARTESIAN_POINT('Ctrl Pts',(78.3877161981791,80.7122045221895,204.452083332377));
#32524=CARTESIAN_POINT('Ctrl Pts',(78.1894917943405,81.388774396239,204.510416665711));
#32525=CARTESIAN_POINT('Ctrl Pts',(77.5044528940591,81.5553919638894,204.568749999044));
#32526=CARTESIAN_POINT('Ctrl Pts',(76.8194139937778,81.7220095315399,204.627083332377));
#32527=CARTESIAN_POINT('Ctrl Pts',(76.332599497335,81.2120572251409,204.685416665711));
#32528=CARTESIAN_POINT('Ctrl Pts',(75.8457850008923,80.7021049187419,204.743749999044));
#32529=CARTESIAN_POINT('Ctrl Pts',(76.0440094047309,80.0255350446925,204.802083332377));
#32530=CARTESIAN_POINT('Ctrl Pts',(76.2422338085695,79.348965170643,204.860416665711));
#32531=CARTESIAN_POINT('Ctrl Pts',(76.9272727088508,79.1823476029926,204.918749999044));
#32532=CARTESIAN_POINT('Ctrl Pts',(77.6123116091322,79.0157300353421,204.977083332377));
#32533=CARTESIAN_POINT('Ctrl Pts',(78.099126105575,79.5256823417411,205.035416665711));
#32534=CARTESIAN_POINT('Ctrl Pts',(78.5859406020177,80.03563464814,205.093749999044));
#32535=CARTESIAN_POINT('Ctrl Pts',(78.3877161981791,80.7122045221895,205.152083332377));
#32536=CARTESIAN_POINT('Ctrl Pts',(78.1894917943405,81.388774396239,205.210416665711));
#32537=CARTESIAN_POINT('Ctrl Pts',(77.5044528940591,81.5553919638894,205.268749999044));
#32538=CARTESIAN_POINT('Ctrl Pts',(76.8194139937778,81.7220095315399,205.327083332377));
#32539=CARTESIAN_POINT('Ctrl Pts',(76.332599497335,81.2120572251409,205.385416665711));
#32540=CARTESIAN_POINT('Ctrl Pts',(75.8457850008923,80.7021049187419,205.443749999044));
#32541=CARTESIAN_POINT('Ctrl Pts',(76.0440094047309,80.0255350446925,205.502083332377));
#32542=CARTESIAN_POINT('Ctrl Pts',(76.2422338085695,79.348965170643,205.560416665711));
#32543=CARTESIAN_POINT('Ctrl Pts',(76.9272727088508,79.1823476029926,205.618749999044));
#32544=CARTESIAN_POINT('Ctrl Pts',(77.6123116091322,79.0157300353421,205.677083332377));
#32545=CARTESIAN_POINT('Ctrl Pts',(78.099126105575,79.5256823417411,205.735416665711));
#32546=CARTESIAN_POINT('Ctrl Pts',(78.5859406020177,80.03563464814,205.793749999044));
#32547=CARTESIAN_POINT('Ctrl Pts',(78.3877161981791,80.7122045221895,205.852083332377));
#32548=CARTESIAN_POINT('Ctrl Pts',(78.1894917943405,81.388774396239,205.910416665711));
#32549=CARTESIAN_POINT('Ctrl Pts',(77.5044528940591,81.5553919638894,205.968749999044));
#32550=CARTESIAN_POINT('Ctrl Pts',(76.8194139937778,81.7220095315399,206.027083332377));
#32551=CARTESIAN_POINT('Ctrl Pts',(76.332599497335,81.2120572251409,206.085416665711));
#32552=CARTESIAN_POINT('Ctrl Pts',(75.8457850008923,80.7021049187419,206.143749999044));
#32553=CARTESIAN_POINT('Ctrl Pts',(76.0440094047309,80.0255350446925,206.202083332377));
#32554=CARTESIAN_POINT('Ctrl Pts',(76.2422338085695,79.348965170643,206.260416665711));
#32555=CARTESIAN_POINT('Ctrl Pts',(76.9272727088508,79.1823476029926,206.318749999044));
#32556=CARTESIAN_POINT('Ctrl Pts',(77.6123116091322,79.0157300353421,206.377083332377));
#32557=CARTESIAN_POINT('Ctrl Pts',(78.099126105575,79.5256823417411,206.435416665711));
#32558=CARTESIAN_POINT('Ctrl Pts',(78.5859406020177,80.03563464814,206.493749999044));
#32559=CARTESIAN_POINT('Ctrl Pts',(78.3877161981791,80.7122045221895,206.552083332377));
#32560=CARTESIAN_POINT('Ctrl Pts',(78.1894917943405,81.3887743962389,206.610416665711));
#32561=CARTESIAN_POINT('Ctrl Pts',(77.5044528940591,81.5553919638894,206.668749999044));
#32562=CARTESIAN_POINT('Ctrl Pts',(76.8194139937778,81.7220095315399,206.727083332378));
#32563=CARTESIAN_POINT('Ctrl Pts',(76.332599497335,81.2120572251409,206.785416665711));
#32564=CARTESIAN_POINT('Ctrl Pts',(75.8457850008923,80.7021049187419,206.843749999044));
#32565=CARTESIAN_POINT('Ctrl Pts',(76.0440094047309,80.0255350446925,206.902083332377));
#32566=CARTESIAN_POINT('Ctrl Pts',(76.2422338085695,79.348965170643,206.960416665711));
#32567=CARTESIAN_POINT('Ctrl Pts',(76.9272727088508,79.1823476029926,207.018749999044));
#32568=CARTESIAN_POINT('Ctrl Pts',(77.6123116091322,79.0157300353421,207.077083332377));
#32569=CARTESIAN_POINT('Ctrl Pts',(78.099126105575,79.5256823417411,207.135416665711));
#32570=CARTESIAN_POINT('Ctrl Pts',(78.5859406020177,80.03563464814,207.193749999044));
#32571=CARTESIAN_POINT('Ctrl Pts',(78.3877161981791,80.7122045221895,207.252083332377));
#32572=CARTESIAN_POINT('Ctrl Pts',(78.1894917943405,81.3887743962389,207.310416665711));
#32573=CARTESIAN_POINT('Ctrl Pts',(77.5044528940591,81.5553919638894,207.368749999044));
#32574=CARTESIAN_POINT('Ctrl Pts',(76.8194139937778,81.7220095315399,207.427083332377));
#32575=CARTESIAN_POINT('Ctrl Pts',(76.332599497335,81.2120572251409,207.485416665711));
#32576=CARTESIAN_POINT('Ctrl Pts',(75.8457850008923,80.7021049187419,207.543749999044));
#32577=CARTESIAN_POINT('Ctrl Pts',(76.0440094047309,80.0255350446925,207.602083332377));
#32578=CARTESIAN_POINT('Ctrl Pts',(76.2422338085695,79.348965170643,207.660416665711));
#32579=CARTESIAN_POINT('Ctrl Pts',(76.9272727088508,79.1823476029926,207.718749999044));
#32580=CARTESIAN_POINT('Ctrl Pts',(77.6123116091322,79.0157300353421,207.777083332377));
#32581=CARTESIAN_POINT('Ctrl Pts',(78.0991261055749,79.5256823417411,207.835416665711));
#32582=CARTESIAN_POINT('Ctrl Pts',(78.5859406020177,80.03563464814,207.893749999044));
#32583=CARTESIAN_POINT('Ctrl Pts',(78.3877161981791,80.7122045221895,207.952083332377));
#32584=CARTESIAN_POINT('Ctrl Pts',(78.1894917943405,81.3887743962389,208.010416665711));
#32585=CARTESIAN_POINT('Ctrl Pts',(77.5044528940591,81.5553919638894,208.068749999044));
#32586=CARTESIAN_POINT('Ctrl Pts',(76.8194139937778,81.7220095315399,208.127083332377));
#32587=CARTESIAN_POINT('Ctrl Pts',(76.332599497335,81.2120572251409,208.185416665711));
#32588=CARTESIAN_POINT('Ctrl Pts',(75.8457850008923,80.7021049187419,208.243749999044));
#32589=CARTESIAN_POINT('Ctrl Pts',(76.0440094047309,80.0255350446925,208.302083332377));
#32590=CARTESIAN_POINT('Ctrl Pts',(76.2422338085695,79.348965170643,208.360416665711));
#32591=CARTESIAN_POINT('Ctrl Pts',(76.9272727088508,79.1823476029926,208.418749999044));
#32592=CARTESIAN_POINT('Ctrl Pts',(77.6123116091322,79.0157300353421,208.477083332377));
#32593=CARTESIAN_POINT('Ctrl Pts',(78.0991261055749,79.5256823417411,208.535416665711));
#32594=CARTESIAN_POINT('Ctrl Pts',(78.5859406020177,80.03563464814,208.593749999044));
#32595=CARTESIAN_POINT('Ctrl Pts',(78.3877161981791,80.7122045221895,208.652083332377));
#32596=CARTESIAN_POINT('Ctrl Pts',(78.1894917943405,81.3887743962389,208.710416665711));
#32597=CARTESIAN_POINT('Ctrl Pts',(77.5044528940591,81.5553919638894,208.768749999044));
#32598=CARTESIAN_POINT('Ctrl Pts',(76.8194139937778,81.7220095315399,208.827083332377));
#32599=CARTESIAN_POINT('Ctrl Pts',(76.332599497335,81.2120572251409,208.885416665711));
#32600=CARTESIAN_POINT('Ctrl Pts',(75.8457850008923,80.7021049187419,208.943749999044));
#32601=CARTESIAN_POINT('Ctrl Pts',(76.0440094047309,80.0255350446925,209.002083332377));
#32602=CARTESIAN_POINT('Ctrl Pts',(76.2422338085695,79.348965170643,209.060416665711));
#32603=CARTESIAN_POINT('Ctrl Pts',(76.9272727088508,79.1823476029926,209.118749999044));
#32604=CARTESIAN_POINT('Ctrl Pts',(77.6123116091322,79.0157300353421,209.177083332377));
#32605=CARTESIAN_POINT('Ctrl Pts',(78.0991261055749,79.5256823417411,209.235416665711));
#32606=CARTESIAN_POINT('Ctrl Pts',(78.5859406020177,80.03563464814,209.293749999044));
#32607=CARTESIAN_POINT('Ctrl Pts',(78.3877161981791,80.7122045221895,209.352083332377));
#32608=CARTESIAN_POINT('Ctrl Pts',(78.1894917943405,81.3887743962389,209.410416665711));
#32609=CARTESIAN_POINT('Ctrl Pts',(77.5044528940591,81.5553919638894,209.468749999044));
#32610=CARTESIAN_POINT('Ctrl Pts',(76.8194139937778,81.7220095315399,209.527083332378));
#32611=CARTESIAN_POINT('Ctrl Pts',(76.332599497335,81.2120572251409,209.585416665711));
#32612=CARTESIAN_POINT('Ctrl Pts',(75.8457850008923,80.7021049187419,209.643749999044));
#32613=CARTESIAN_POINT('Ctrl Pts',(76.0440094047309,80.0255350446925,209.702083332377));
#32614=CARTESIAN_POINT('Ctrl Pts',(76.2422338085695,79.348965170643,209.760416665711));
#32615=CARTESIAN_POINT('Ctrl Pts',(76.9272727088508,79.1823476029926,209.818749999044));
#32616=CARTESIAN_POINT('Ctrl Pts',(77.6123116091322,79.0157300353421,209.877083332377));
#32617=CARTESIAN_POINT('Ctrl Pts',(78.0991261055749,79.5256823417411,209.935416665711));
#32618=CARTESIAN_POINT('Ctrl Pts',(78.5859406020177,80.03563464814,209.993749999044));
#32619=CARTESIAN_POINT('Ctrl Pts',(78.3877161981791,80.7122045221895,210.052083332377));
#32620=CARTESIAN_POINT('Ctrl Pts',(78.1894917943405,81.3887743962389,210.110416665711));
#32621=CARTESIAN_POINT('Ctrl Pts',(77.5044528940591,81.5553919638894,210.168749999044));
#32622=CARTESIAN_POINT('Ctrl Pts',(76.8194139937778,81.7220095315399,210.227083332377));
#32623=CARTESIAN_POINT('Ctrl Pts',(76.332599497335,81.2120572251409,210.285416665711));
#32624=CARTESIAN_POINT('Ctrl Pts',(75.8457850008923,80.7021049187419,210.343749999044));
#32625=CARTESIAN_POINT('Ctrl Pts',(76.0440094047309,80.0255350446925,210.402083332377));
#32626=CARTESIAN_POINT('Ctrl Pts',(76.2422338085695,79.348965170643,210.460416665711));
#32627=CARTESIAN_POINT('Ctrl Pts',(76.9272727088508,79.1823476029926,210.518749999044));
#32628=CARTESIAN_POINT('Ctrl Pts',(77.6123116091322,79.0157300353421,210.577083332377));
#32629=CARTESIAN_POINT('Ctrl Pts',(78.0991261055749,79.5256823417411,210.635416665711));
#32630=CARTESIAN_POINT('Ctrl Pts',(78.5859406020177,80.03563464814,210.693749999044));
#32631=CARTESIAN_POINT('Ctrl Pts',(78.3877161981791,80.7122045221895,210.752083332377));
#32632=CARTESIAN_POINT('Ctrl Pts',(78.1894917943405,81.3887743962389,210.810416665711));
#32633=CARTESIAN_POINT('Ctrl Pts',(77.5044528940591,81.5553919638894,210.868749999044));
#32634=CARTESIAN_POINT('Ctrl Pts',(76.8194139937778,81.7220095315399,210.927083332377));
#32635=CARTESIAN_POINT('Ctrl Pts',(76.332599497335,81.2120572251409,210.985416665711));
#32636=CARTESIAN_POINT('Ctrl Pts',(75.8457850008923,80.7021049187419,211.043749999044));
#32637=CARTESIAN_POINT('Ctrl Pts',(76.0440094047309,80.0255350446925,211.102083332377));
#32638=CARTESIAN_POINT('Ctrl Pts',(76.2422338085695,79.348965170643,211.160416665711));
#32639=CARTESIAN_POINT('Ctrl Pts',(76.9272727088508,79.1823476029925,211.218749999044));
#32640=CARTESIAN_POINT('Ctrl Pts',(77.6123116091322,79.0157300353421,211.277083332377));
#32641=CARTESIAN_POINT('Ctrl Pts',(78.0991261055749,79.5256823417411,211.335416665711));
#32642=CARTESIAN_POINT('Ctrl Pts',(78.5859406020177,80.03563464814,211.393749999044));
#32643=CARTESIAN_POINT('Ctrl Pts',(78.3877161981791,80.7122045221895,211.452083332377));
#32644=CARTESIAN_POINT('Ctrl Pts',(78.1894917943405,81.3887743962389,211.510416665711));
#32645=CARTESIAN_POINT('Ctrl Pts',(77.5044528940591,81.5553919638894,211.568749999044));
#32646=CARTESIAN_POINT('Ctrl Pts',(76.8194139937778,81.7220095315399,211.627083332377));
#32647=CARTESIAN_POINT('Ctrl Pts',(76.332599497335,81.2120572251409,211.685416665711));
#32648=CARTESIAN_POINT('Ctrl Pts',(75.8457850008923,80.7021049187419,211.743749999044));
#32649=CARTESIAN_POINT('Ctrl Pts',(76.0440094047309,80.0255350446925,211.802083332377));
#32650=CARTESIAN_POINT('Ctrl Pts',(76.2422338085695,79.348965170643,211.860416665711));
#32651=CARTESIAN_POINT('Ctrl Pts',(76.9272727088508,79.1823476029925,211.918749999044));
#32652=CARTESIAN_POINT('Ctrl Pts',(76.8377292359511,78.8141945740679,197.7));
#32653=CARTESIAN_POINT('Ctrl Pts',(77.7353213865851,78.5958790582346,197.758333333333));
#32654=CARTESIAN_POINT('Ctrl Pts',(78.3731842446541,79.2640589050045,197.816666666667));
#32655=CARTESIAN_POINT('Ctrl Pts',(79.011047102723,79.9322387517744,197.875));
#32656=CARTESIAN_POINT('Ctrl Pts',(78.7513178101579,80.8187341143776,197.933333333333));
#32657=CARTESIAN_POINT('Ctrl Pts',(78.4915885175929,81.7052294769809,197.991666666667));
#32658=CARTESIAN_POINT('Ctrl Pts',(77.5939963669589,81.9235449928141,198.05));
#32659=CARTESIAN_POINT('Ctrl Pts',(76.6964042163248,82.1418605086474,198.108333333333));
#32660=CARTESIAN_POINT('Ctrl Pts',(76.0585413582559,81.4736806618775,198.166666666667));
#32661=CARTESIAN_POINT('Ctrl Pts',(75.420678500187,80.8055008151076,198.225));
#32662=CARTESIAN_POINT('Ctrl Pts',(75.6804077927521,79.9190054525044,198.283333333333));
#32663=CARTESIAN_POINT('Ctrl Pts',(75.9401370853171,79.0325100899012,198.341666666667));
#32664=CARTESIAN_POINT('Ctrl Pts',(76.8377292359511,78.8141945740679,198.4));
#32665=CARTESIAN_POINT('Ctrl Pts',(77.7353213865851,78.5958790582346,198.458333333333));
#32666=CARTESIAN_POINT('Ctrl Pts',(78.3731842446541,79.2640589050045,198.516666666667));
#32667=CARTESIAN_POINT('Ctrl Pts',(79.011047102723,79.9322387517744,198.575));
#32668=CARTESIAN_POINT('Ctrl Pts',(78.7513178101579,80.8187341143776,198.633333333333));
#32669=CARTESIAN_POINT('Ctrl Pts',(78.4915885175929,81.7052294769809,198.691666666667));
#32670=CARTESIAN_POINT('Ctrl Pts',(77.5939963669589,81.9235449928141,198.75));
#32671=CARTESIAN_POINT('Ctrl Pts',(76.6964042163248,82.1418605086474,198.808333333333));
#32672=CARTESIAN_POINT('Ctrl Pts',(76.0585413582559,81.4736806618775,198.866666666667));
#32673=CARTESIAN_POINT('Ctrl Pts',(75.420678500187,80.8055008151076,198.925));
#32674=CARTESIAN_POINT('Ctrl Pts',(75.6804077927521,79.9190054525044,198.983333333333));
#32675=CARTESIAN_POINT('Ctrl Pts',(75.9401370853171,79.0325100899012,199.041666666667));
#32676=CARTESIAN_POINT('Ctrl Pts',(76.8377292359511,78.8141945740679,199.1));
#32677=CARTESIAN_POINT('Ctrl Pts',(77.7353213865851,78.5958790582346,199.158333333333));
#32678=CARTESIAN_POINT('Ctrl Pts',(78.3731842446541,79.2640589050045,199.216666666667));
#32679=CARTESIAN_POINT('Ctrl Pts',(79.011047102723,79.9322387517744,199.275));
#32680=CARTESIAN_POINT('Ctrl Pts',(78.7513178101579,80.8187341143776,199.333333333333));
#32681=CARTESIAN_POINT('Ctrl Pts',(78.4915885175929,81.7052294769809,199.391666666667));
#32682=CARTESIAN_POINT('Ctrl Pts',(77.5939963669589,81.9235449928141,199.45));
#32683=CARTESIAN_POINT('Ctrl Pts',(76.6964042163248,82.1418605086474,199.508333333333));
#32684=CARTESIAN_POINT('Ctrl Pts',(76.0585413582559,81.4736806618775,199.566666666667));
#32685=CARTESIAN_POINT('Ctrl Pts',(75.420678500187,80.8055008151076,199.625));
#32686=CARTESIAN_POINT('Ctrl Pts',(75.6804077927521,79.9190054525044,199.683333333333));
#32687=CARTESIAN_POINT('Ctrl Pts',(75.9401370853171,79.0325100899012,199.741666666667));
#32688=CARTESIAN_POINT('Ctrl Pts',(76.8377292359511,78.8141945740679,199.8));
#32689=CARTESIAN_POINT('Ctrl Pts',(77.7353213865851,78.5958790582346,199.858333333333));
#32690=CARTESIAN_POINT('Ctrl Pts',(78.3731842446541,79.2640589050045,199.916666666667));
#32691=CARTESIAN_POINT('Ctrl Pts',(79.011047102723,79.9322387517744,199.975));
#32692=CARTESIAN_POINT('Ctrl Pts',(78.7513178101579,80.8187341143776,200.033333333333));
#32693=CARTESIAN_POINT('Ctrl Pts',(78.4915885175929,81.7052294769809,200.091666666667));
#32694=CARTESIAN_POINT('Ctrl Pts',(77.5939963669589,81.9235449928141,200.15));
#32695=CARTESIAN_POINT('Ctrl Pts',(76.6964042163248,82.1418605086474,200.208333333333));
#32696=CARTESIAN_POINT('Ctrl Pts',(76.0585413582559,81.4736806618775,200.266666666667));
#32697=CARTESIAN_POINT('Ctrl Pts',(75.420678500187,80.8055008151076,200.325));
#32698=CARTESIAN_POINT('Ctrl Pts',(75.680407792752,79.9190054525044,200.383333333333));
#32699=CARTESIAN_POINT('Ctrl Pts',(75.9401370853171,79.0325100899012,200.441666666667));
#32700=CARTESIAN_POINT('Ctrl Pts',(76.8377292359511,78.8141945740679,200.5));
#32701=CARTESIAN_POINT('Ctrl Pts',(77.7353213865851,78.5958790582346,200.558333333333));
#32702=CARTESIAN_POINT('Ctrl Pts',(78.3731842446541,79.2640589050045,200.616666666667));
#32703=CARTESIAN_POINT('Ctrl Pts',(79.011047102723,79.9322387517744,200.675));
#32704=CARTESIAN_POINT('Ctrl Pts',(78.7513178101579,80.8187341143776,200.733333333333));
#32705=CARTESIAN_POINT('Ctrl Pts',(78.4915885175929,81.7052294769809,200.791666666667));
#32706=CARTESIAN_POINT('Ctrl Pts',(77.5939963669589,81.9235449928141,200.85));
#32707=CARTESIAN_POINT('Ctrl Pts',(76.6964042163248,82.1418605086474,200.908333333333));
#32708=CARTESIAN_POINT('Ctrl Pts',(76.0585413582559,81.4736806618775,200.966666666667));
#32709=CARTESIAN_POINT('Ctrl Pts',(75.420678500187,80.8055008151076,201.025));
#32710=CARTESIAN_POINT('Ctrl Pts',(75.680407792752,79.9190054525044,201.083333333333));
#32711=CARTESIAN_POINT('Ctrl Pts',(75.9401370853171,79.0325100899012,201.141666666667));
#32712=CARTESIAN_POINT('Ctrl Pts',(76.8377292359511,78.8141945740679,201.2));
#32713=CARTESIAN_POINT('Ctrl Pts',(77.7353213865851,78.5958790582346,201.258333333333));
#32714=CARTESIAN_POINT('Ctrl Pts',(78.3731842446541,79.2640589050045,201.316666666667));
#32715=CARTESIAN_POINT('Ctrl Pts',(79.011047102723,79.9322387517744,201.375));
#32716=CARTESIAN_POINT('Ctrl Pts',(78.7513178101579,80.8187341143776,201.433333333333));
#32717=CARTESIAN_POINT('Ctrl Pts',(78.4915885175929,81.7052294769809,201.491666666667));
#32718=CARTESIAN_POINT('Ctrl Pts',(77.5939963669589,81.9235449928141,201.55));
#32719=CARTESIAN_POINT('Ctrl Pts',(76.6964042163248,82.1418605086474,201.608333333333));
#32720=CARTESIAN_POINT('Ctrl Pts',(76.0585413582559,81.4736806618775,201.666666666667));
#32721=CARTESIAN_POINT('Ctrl Pts',(75.420678500187,80.8055008151076,201.725));
#32722=CARTESIAN_POINT('Ctrl Pts',(75.680407792752,79.9190054525044,201.783333333333));
#32723=CARTESIAN_POINT('Ctrl Pts',(75.9401370853171,79.0325100899012,201.841666666667));
#32724=CARTESIAN_POINT('Ctrl Pts',(76.8377292359511,78.8141945740679,201.9));
#32725=CARTESIAN_POINT('Ctrl Pts',(77.7353213865851,78.5958790582346,201.958333333333));
#32726=CARTESIAN_POINT('Ctrl Pts',(78.3731842446541,79.2640589050045,202.016666666667));
#32727=CARTESIAN_POINT('Ctrl Pts',(79.011047102723,79.9322387517744,202.075));
#32728=CARTESIAN_POINT('Ctrl Pts',(78.7513178101579,80.8187341143776,202.133333333333));
#32729=CARTESIAN_POINT('Ctrl Pts',(78.4915885175929,81.7052294769808,202.191666666667));
#32730=CARTESIAN_POINT('Ctrl Pts',(77.5939963669589,81.9235449928141,202.25));
#32731=CARTESIAN_POINT('Ctrl Pts',(76.6964042163248,82.1418605086474,202.308333333333));
#32732=CARTESIAN_POINT('Ctrl Pts',(76.0585413582559,81.4736806618775,202.366666666667));
#32733=CARTESIAN_POINT('Ctrl Pts',(75.420678500187,80.8055008151076,202.425));
#32734=CARTESIAN_POINT('Ctrl Pts',(75.680407792752,79.9190054525044,202.483333333333));
#32735=CARTESIAN_POINT('Ctrl Pts',(75.9401370853171,79.0325100899012,202.541666666667));
#32736=CARTESIAN_POINT('Ctrl Pts',(76.8377292359511,78.8141945740679,202.6));
#32737=CARTESIAN_POINT('Ctrl Pts',(77.7353213865851,78.5958790582346,202.658333333333));
#32738=CARTESIAN_POINT('Ctrl Pts',(78.3731842446541,79.2640589050045,202.716666666667));
#32739=CARTESIAN_POINT('Ctrl Pts',(79.011047102723,79.9322387517744,202.775));
#32740=CARTESIAN_POINT('Ctrl Pts',(78.7513178101579,80.8187341143776,202.833333333333));
#32741=CARTESIAN_POINT('Ctrl Pts',(78.4915885175929,81.7052294769808,202.891666666667));
#32742=CARTESIAN_POINT('Ctrl Pts',(77.5939963669589,81.9235449928141,202.95));
#32743=CARTESIAN_POINT('Ctrl Pts',(76.6964042163248,82.1418605086474,203.008333333333));
#32744=CARTESIAN_POINT('Ctrl Pts',(76.0585413582559,81.4736806618775,203.066666666667));
#32745=CARTESIAN_POINT('Ctrl Pts',(75.420678500187,80.8055008151076,203.125));
#32746=CARTESIAN_POINT('Ctrl Pts',(75.680407792752,79.9190054525044,203.183333333333));
#32747=CARTESIAN_POINT('Ctrl Pts',(75.9401370853171,79.0325100899012,203.241666666667));
#32748=CARTESIAN_POINT('Ctrl Pts',(76.8377292359511,78.8141945740679,203.3));
#32749=CARTESIAN_POINT('Ctrl Pts',(77.7353213865851,78.5958790582346,203.358333333333));
#32750=CARTESIAN_POINT('Ctrl Pts',(78.3731842446541,79.2640589050045,203.416666666667));
#32751=CARTESIAN_POINT('Ctrl Pts',(79.011047102723,79.9322387517744,203.475));
#32752=CARTESIAN_POINT('Ctrl Pts',(78.7513178101579,80.8187341143776,203.533333333333));
#32753=CARTESIAN_POINT('Ctrl Pts',(78.4915885175929,81.7052294769808,203.591666666667));
#32754=CARTESIAN_POINT('Ctrl Pts',(77.5939963669589,81.9235449928141,203.65));
#32755=CARTESIAN_POINT('Ctrl Pts',(76.6964042163248,82.1418605086474,203.708333333333));
#32756=CARTESIAN_POINT('Ctrl Pts',(76.0585413582559,81.4736806618775,203.766666666667));
#32757=CARTESIAN_POINT('Ctrl Pts',(75.420678500187,80.8055008151076,203.825));
#32758=CARTESIAN_POINT('Ctrl Pts',(75.680407792752,79.9190054525044,203.883333333333));
#32759=CARTESIAN_POINT('Ctrl Pts',(75.9401370853171,79.0325100899012,203.941666666667));
#32760=CARTESIAN_POINT('Ctrl Pts',(76.8377292359511,78.8141945740679,204.));
#32761=CARTESIAN_POINT('Ctrl Pts',(77.7353213865851,78.5958790582346,204.058333333333));
#32762=CARTESIAN_POINT('Ctrl Pts',(78.3731842446541,79.2640589050045,204.116666666667));
#32763=CARTESIAN_POINT('Ctrl Pts',(79.011047102723,79.9322387517744,204.175));
#32764=CARTESIAN_POINT('Ctrl Pts',(78.7513178101579,80.8187341143776,204.233333333333));
#32765=CARTESIAN_POINT('Ctrl Pts',(78.4915885175929,81.7052294769808,204.291666666667));
#32766=CARTESIAN_POINT('Ctrl Pts',(77.5939963669589,81.9235449928141,204.35));
#32767=CARTESIAN_POINT('Ctrl Pts',(76.6964042163248,82.1418605086474,204.408333333333));
#32768=CARTESIAN_POINT('Ctrl Pts',(76.0585413582559,81.4736806618775,204.466666666667));
#32769=CARTESIAN_POINT('Ctrl Pts',(75.420678500187,80.8055008151076,204.525));
#32770=CARTESIAN_POINT('Ctrl Pts',(75.680407792752,79.9190054525044,204.583333333333));
#32771=CARTESIAN_POINT('Ctrl Pts',(75.9401370853171,79.0325100899012,204.641666666667));
#32772=CARTESIAN_POINT('Ctrl Pts',(76.8377292359511,78.8141945740679,204.7));
#32773=CARTESIAN_POINT('Ctrl Pts',(77.7353213865851,78.5958790582346,204.758333333333));
#32774=CARTESIAN_POINT('Ctrl Pts',(78.3731842446541,79.2640589050045,204.816666666667));
#32775=CARTESIAN_POINT('Ctrl Pts',(79.011047102723,79.9322387517744,204.875));
#32776=CARTESIAN_POINT('Ctrl Pts',(78.7513178101579,80.8187341143776,204.933333333333));
#32777=CARTESIAN_POINT('Ctrl Pts',(78.4915885175928,81.7052294769808,204.991666666667));
#32778=CARTESIAN_POINT('Ctrl Pts',(77.5939963669589,81.9235449928141,205.05));
#32779=CARTESIAN_POINT('Ctrl Pts',(76.6964042163248,82.1418605086474,205.108333333333));
#32780=CARTESIAN_POINT('Ctrl Pts',(76.0585413582559,81.4736806618775,205.166666666667));
#32781=CARTESIAN_POINT('Ctrl Pts',(75.420678500187,80.8055008151076,205.225));
#32782=CARTESIAN_POINT('Ctrl Pts',(75.680407792752,79.9190054525044,205.283333333333));
#32783=CARTESIAN_POINT('Ctrl Pts',(75.9401370853171,79.0325100899011,205.341666666667));
#32784=CARTESIAN_POINT('Ctrl Pts',(76.8377292359511,78.8141945740679,205.4));
#32785=CARTESIAN_POINT('Ctrl Pts',(77.7353213865851,78.5958790582346,205.458333333333));
#32786=CARTESIAN_POINT('Ctrl Pts',(78.3731842446541,79.2640589050045,205.516666666667));
#32787=CARTESIAN_POINT('Ctrl Pts',(79.011047102723,79.9322387517744,205.575));
#32788=CARTESIAN_POINT('Ctrl Pts',(78.7513178101579,80.8187341143776,205.633333333333));
#32789=CARTESIAN_POINT('Ctrl Pts',(78.4915885175928,81.7052294769808,205.691666666667));
#32790=CARTESIAN_POINT('Ctrl Pts',(77.5939963669589,81.9235449928141,205.75));
#32791=CARTESIAN_POINT('Ctrl Pts',(76.6964042163248,82.1418605086474,205.808333333333));
#32792=CARTESIAN_POINT('Ctrl Pts',(76.0585413582559,81.4736806618775,205.866666666667));
#32793=CARTESIAN_POINT('Ctrl Pts',(75.420678500187,80.8055008151076,205.925));
#32794=CARTESIAN_POINT('Ctrl Pts',(75.680407792752,79.9190054525044,205.983333333333));
#32795=CARTESIAN_POINT('Ctrl Pts',(75.9401370853171,79.0325100899011,206.041666666667));
#32796=CARTESIAN_POINT('Ctrl Pts',(76.8377292359511,78.8141945740679,206.1));
#32797=CARTESIAN_POINT('Ctrl Pts',(77.7353213865851,78.5958790582346,206.158333333333));
#32798=CARTESIAN_POINT('Ctrl Pts',(78.3731842446541,79.2640589050045,206.216666666667));
#32799=CARTESIAN_POINT('Ctrl Pts',(79.011047102723,79.9322387517744,206.275));
#32800=CARTESIAN_POINT('Ctrl Pts',(78.7513178101579,80.8187341143776,206.333333333333));
#32801=CARTESIAN_POINT('Ctrl Pts',(78.4915885175928,81.7052294769808,206.391666666667));
#32802=CARTESIAN_POINT('Ctrl Pts',(77.5939963669589,81.9235449928141,206.45));
#32803=CARTESIAN_POINT('Ctrl Pts',(76.6964042163248,82.1418605086474,206.508333333333));
#32804=CARTESIAN_POINT('Ctrl Pts',(76.0585413582559,81.4736806618775,206.566666666667));
#32805=CARTESIAN_POINT('Ctrl Pts',(75.420678500187,80.8055008151076,206.625));
#32806=CARTESIAN_POINT('Ctrl Pts',(75.680407792752,79.9190054525043,206.683333333333));
#32807=CARTESIAN_POINT('Ctrl Pts',(75.9401370853171,79.0325100899011,206.741666666667));
#32808=CARTESIAN_POINT('Ctrl Pts',(76.8377292359511,78.8141945740679,206.8));
#32809=CARTESIAN_POINT('Ctrl Pts',(77.7353213865851,78.5958790582346,206.858333333333));
#32810=CARTESIAN_POINT('Ctrl Pts',(78.3731842446541,79.2640589050045,206.916666666667));
#32811=CARTESIAN_POINT('Ctrl Pts',(79.011047102723,79.9322387517744,206.975));
#32812=CARTESIAN_POINT('Ctrl Pts',(78.7513178101579,80.8187341143776,207.033333333333));
#32813=CARTESIAN_POINT('Ctrl Pts',(78.4915885175928,81.7052294769808,207.091666666667));
#32814=CARTESIAN_POINT('Ctrl Pts',(77.5939963669589,81.9235449928141,207.15));
#32815=CARTESIAN_POINT('Ctrl Pts',(76.6964042163248,82.1418605086474,207.208333333333));
#32816=CARTESIAN_POINT('Ctrl Pts',(76.0585413582559,81.4736806618775,207.266666666667));
#32817=CARTESIAN_POINT('Ctrl Pts',(75.420678500187,80.8055008151075,207.325));
#32818=CARTESIAN_POINT('Ctrl Pts',(75.680407792752,79.9190054525043,207.383333333333));
#32819=CARTESIAN_POINT('Ctrl Pts',(75.9401370853171,79.0325100899011,207.441666666667));
#32820=CARTESIAN_POINT('Ctrl Pts',(76.8377292359511,78.8141945740679,207.5));
#32821=CARTESIAN_POINT('Ctrl Pts',(77.7353213865851,78.5958790582346,207.558333333333));
#32822=CARTESIAN_POINT('Ctrl Pts',(78.3731842446541,79.2640589050045,207.616666666667));
#32823=CARTESIAN_POINT('Ctrl Pts',(79.011047102723,79.9322387517744,207.675));
#32824=CARTESIAN_POINT('Ctrl Pts',(78.7513178101579,80.8187341143776,207.733333333333));
#32825=CARTESIAN_POINT('Ctrl Pts',(78.4915885175928,81.7052294769808,207.791666666667));
#32826=CARTESIAN_POINT('Ctrl Pts',(77.5939963669589,81.9235449928141,207.85));
#32827=CARTESIAN_POINT('Ctrl Pts',(76.6964042163248,82.1418605086474,207.908333333333));
#32828=CARTESIAN_POINT('Ctrl Pts',(76.0585413582559,81.4736806618775,207.966666666667));
#32829=CARTESIAN_POINT('Ctrl Pts',(75.420678500187,80.8055008151075,208.025));
#32830=CARTESIAN_POINT('Ctrl Pts',(75.680407792752,79.9190054525043,208.083333333333));
#32831=CARTESIAN_POINT('Ctrl Pts',(75.9401370853171,79.0325100899011,208.141666666667));
#32832=CARTESIAN_POINT('Ctrl Pts',(76.8377292359511,78.8141945740679,208.2));
#32833=CARTESIAN_POINT('Ctrl Pts',(77.7353213865851,78.5958790582346,208.258333333333));
#32834=CARTESIAN_POINT('Ctrl Pts',(78.3731842446541,79.2640589050045,208.316666666667));
#32835=CARTESIAN_POINT('Ctrl Pts',(79.011047102723,79.9322387517744,208.375));
#32836=CARTESIAN_POINT('Ctrl Pts',(78.7513178101579,80.8187341143776,208.433333333333));
#32837=CARTESIAN_POINT('Ctrl Pts',(78.4915885175928,81.7052294769808,208.491666666667));
#32838=CARTESIAN_POINT('Ctrl Pts',(77.5939963669589,81.9235449928141,208.55));
#32839=CARTESIAN_POINT('Ctrl Pts',(76.6964042163248,82.1418605086474,208.608333333333));
#32840=CARTESIAN_POINT('Ctrl Pts',(76.0585413582559,81.4736806618775,208.666666666667));
#32841=CARTESIAN_POINT('Ctrl Pts',(75.420678500187,80.8055008151075,208.725));
#32842=CARTESIAN_POINT('Ctrl Pts',(75.680407792752,79.9190054525043,208.783333333333));
#32843=CARTESIAN_POINT('Ctrl Pts',(75.9401370853171,79.0325100899011,208.841666666667));
#32844=CARTESIAN_POINT('Ctrl Pts',(76.8377292359511,78.8141945740679,208.9));
#32845=CARTESIAN_POINT('Ctrl Pts',(77.7353213865851,78.5958790582346,208.958333333333));
#32846=CARTESIAN_POINT('Ctrl Pts',(78.3731842446541,79.2640589050045,209.016666666667));
#32847=CARTESIAN_POINT('Ctrl Pts',(79.011047102723,79.9322387517744,209.075));
#32848=CARTESIAN_POINT('Ctrl Pts',(78.7513178101579,80.8187341143776,209.133333333333));
#32849=CARTESIAN_POINT('Ctrl Pts',(78.4915885175928,81.7052294769808,209.191666666667));
#32850=CARTESIAN_POINT('Ctrl Pts',(77.5939963669589,81.9235449928141,209.25));
#32851=CARTESIAN_POINT('Ctrl Pts',(76.6964042163248,82.1418605086474,209.308333333333));
#32852=CARTESIAN_POINT('Ctrl Pts',(76.0585413582559,81.4736806618775,209.366666666667));
#32853=CARTESIAN_POINT('Ctrl Pts',(75.420678500187,80.8055008151075,209.425));
#32854=CARTESIAN_POINT('Ctrl Pts',(75.680407792752,79.9190054525043,209.483333333333));
#32855=CARTESIAN_POINT('Ctrl Pts',(75.9401370853171,79.0325100899011,209.541666666667));
#32856=CARTESIAN_POINT('Ctrl Pts',(76.8377292359511,78.8141945740679,209.6));
#32857=CARTESIAN_POINT('Ctrl Pts',(77.7353213865851,78.5958790582346,209.658333333333));
#32858=CARTESIAN_POINT('Ctrl Pts',(78.3731842446541,79.2640589050045,209.716666666667));
#32859=CARTESIAN_POINT('Ctrl Pts',(79.011047102723,79.9322387517744,209.775));
#32860=CARTESIAN_POINT('Ctrl Pts',(78.7513178101579,80.8187341143776,209.833333333333));
#32861=CARTESIAN_POINT('Ctrl Pts',(78.4915885175928,81.7052294769808,209.891666666667));
#32862=CARTESIAN_POINT('Ctrl Pts',(77.5939963669589,81.9235449928141,209.95));
#32863=CARTESIAN_POINT('Ctrl Pts',(76.6964042163248,82.1418605086474,210.008333333333));
#32864=CARTESIAN_POINT('Ctrl Pts',(76.0585413582559,81.4736806618775,210.066666666667));
#32865=CARTESIAN_POINT('Ctrl Pts',(75.420678500187,80.8055008151075,210.125));
#32866=CARTESIAN_POINT('Ctrl Pts',(75.680407792752,79.9190054525043,210.183333333333));
#32867=CARTESIAN_POINT('Ctrl Pts',(75.9401370853171,79.0325100899011,210.241666666667));
#32868=CARTESIAN_POINT('Ctrl Pts',(76.8377292359511,78.8141945740679,210.3));
#32869=CARTESIAN_POINT('Ctrl Pts',(77.7353213865851,78.5958790582346,210.358333333333));
#32870=CARTESIAN_POINT('Ctrl Pts',(78.3731842446541,79.2640589050045,210.416666666667));
#32871=CARTESIAN_POINT('Ctrl Pts',(79.011047102723,79.9322387517744,210.475));
#32872=CARTESIAN_POINT('Ctrl Pts',(78.7513178101579,80.8187341143776,210.533333333333));
#32873=CARTESIAN_POINT('Ctrl Pts',(78.4915885175928,81.7052294769808,210.591666666667));
#32874=CARTESIAN_POINT('Ctrl Pts',(77.5939963669589,81.9235449928141,210.65));
#32875=CARTESIAN_POINT('Ctrl Pts',(76.6964042163248,82.1418605086474,210.708333333333));
#32876=CARTESIAN_POINT('Ctrl Pts',(76.0585413582559,81.4736806618775,210.766666666667));
#32877=CARTESIAN_POINT('Ctrl Pts',(75.420678500187,80.8055008151075,210.825));
#32878=CARTESIAN_POINT('Ctrl Pts',(75.680407792752,79.9190054525043,210.883333333333));
#32879=CARTESIAN_POINT('Ctrl Pts',(75.9401370853171,79.0325100899011,210.941666666667));
#32880=CARTESIAN_POINT('Ctrl Pts',(76.8377292359511,78.8141945740679,211.));
#32881=CARTESIAN_POINT('Ctrl Pts',(77.7353213865851,78.5958790582346,211.058333333333));
#32882=CARTESIAN_POINT('Ctrl Pts',(78.3731842446541,79.2640589050045,211.116666666667));
#32883=CARTESIAN_POINT('Ctrl Pts',(79.011047102723,79.9322387517744,211.175));
#32884=CARTESIAN_POINT('Ctrl Pts',(78.7513178101579,80.8187341143776,211.233333333333));
#32885=CARTESIAN_POINT('Ctrl Pts',(78.4915885175928,81.7052294769808,211.291666666667));
#32886=CARTESIAN_POINT('Ctrl Pts',(77.5939963669589,81.9235449928141,211.35));
#32887=CARTESIAN_POINT('Ctrl Pts',(76.6964042163248,82.1418605086474,211.408333333333));
#32888=CARTESIAN_POINT('Ctrl Pts',(76.0585413582559,81.4736806618775,211.466666666667));
#32889=CARTESIAN_POINT('Ctrl Pts',(75.420678500187,80.8055008151075,211.525));
#32890=CARTESIAN_POINT('Ctrl Pts',(75.680407792752,79.9190054525043,211.583333333333));
#32891=CARTESIAN_POINT('Ctrl Pts',(75.9401370853171,79.0325100899011,211.641666666667));
#32892=CARTESIAN_POINT('Ctrl Pts',(76.8377292359511,78.8141945740679,211.7));
#32893=CARTESIAN_POINT('',(76.8377292359511,78.8141945740679,197.7));
#32894=CARTESIAN_POINT('',(76.882500972401,78.9982710885302,197.809374999522));
#32895=CARTESIAN_POINT('',(76.882500972401,78.9982710885302,211.809374999522));
#32896=CARTESIAN_POINT('Ctrl Pts',(76.8377292359511,78.8141945740678,211.));
#32897=CARTESIAN_POINT('Ctrl Pts',(76.7421956368437,78.837430591622,210.993791397042));
#32898=CARTESIAN_POINT('Ctrl Pts',(76.6488078291848,78.8694683758089,210.987252804374));
#32899=CARTESIAN_POINT('Ctrl Pts',(76.3697606459006,78.9951613331449,210.966206582705));
#32900=CARTESIAN_POINT('Ctrl Pts',(76.1991296043222,79.1161951267954,210.951113087222));
#32901=CARTESIAN_POINT('Ctrl Pts',(75.9100735650893,79.4202005198414,210.920561039534));
#32902=CARTESIAN_POINT('Ctrl Pts',(75.7958364286097,79.6016502668059,210.905399990094));
#32903=CARTESIAN_POINT('Ctrl Pts',(75.6482827813348,79.9896598075252,210.878081571274));
#32904=CARTESIAN_POINT('Ctrl Pts',(75.6128796701455,80.191143614408,210.865215738096));
#32905=CARTESIAN_POINT('Ctrl Pts',(75.6193462602684,80.6035916812702,210.835881909083));
#32906=CARTESIAN_POINT('Ctrl Pts',(75.6638079674599,80.8105491249732,210.82045255689));
#32907=CARTESIAN_POINT('Ctrl Pts',(75.8314666514945,81.1989094692805,210.790047602273));
#32908=CARTESIAN_POINT('Ctrl Pts',(75.9543114774069,81.3758154595951,210.775966565719));
#32909=CARTESIAN_POINT('Ctrl Pts',(76.255656315336,81.6649371807569,210.748952445063));
#32910=CARTESIAN_POINT('Ctrl Pts',(76.4288855612612,81.7768509112186,210.73453628646));
#32911=CARTESIAN_POINT('Ctrl Pts',(76.8153671419507,81.9324155231772,210.70430284673));
#32912=CARTESIAN_POINT('Ctrl Pts',(77.0261552911063,81.9717112472583,210.688747285219));
#32913=CARTESIAN_POINT('Ctrl Pts',(77.4444681194566,81.9657981638116,210.659597004652));
#32914=CARTESIAN_POINT('Ctrl Pts',(77.6478918569701,81.9231498342464,210.647137520362));
#32915=CARTESIAN_POINT('Ctrl Pts',(78.0282269886831,81.762722375082,210.619000254481));
#32916=CARTESIAN_POINT('Ctrl Pts',(78.2013501921092,81.6461904160994,210.604001981035));
#32917=CARTESIAN_POINT('Ctrl Pts',(78.4975778231958,81.3498282284663,210.573456516786));
#32918=CARTESIAN_POINT('Ctrl Pts',(78.6163205365602,81.1712592597555,210.558202877509));
#32919=CARTESIAN_POINT('Ctrl Pts',(78.7735690054945,80.7868720228714,210.530555510445));
#32920=CARTESIAN_POINT('Ctrl Pts',(78.8139767093485,80.5861890491931,210.517937042288));
#32921=CARTESIAN_POINT('Ctrl Pts',(78.8176755362887,80.1740840495194,210.488802697026));
#32922=CARTESIAN_POINT('Ctrl Pts',(78.7785249852346,79.9665967007589,210.473427325777));
#32923=CARTESIAN_POINT('Ctrl Pts',(78.6214269969712,79.5754662289674,210.443008093394));
#32924=CARTESIAN_POINT('Ctrl Pts',(78.503876463604,79.3962335317332,210.428521671259));
#32925=CARTESIAN_POINT('Ctrl Pts',(78.2117293575683,79.1000869433297,210.402007142167));
#32926=CARTESIAN_POINT('Ctrl Pts',(78.0421770439422,78.9836916635366,210.387756398436));
#32927=CARTESIAN_POINT('Ctrl Pts',(77.6613663356015,78.817631266407,210.357704598224));
#32928=CARTESIAN_POINT('Ctrl Pts',(77.4524279876431,78.7723536599372,210.342155838516));
#32929=CARTESIAN_POINT('Ctrl Pts',(77.1047144563197,78.7669488199961,210.317713719403));
#32930=CARTESIAN_POINT('Ctrl Pts',(76.9693379669327,78.7821842362188,210.308553078331));
#32931=CARTESIAN_POINT('Ctrl Pts',(76.8377292359507,78.814194574068,210.3));
#32932=CARTESIAN_POINT('Ctrl Pts',(76.8377292359511,78.8141945740679,197.7));
#32933=CARTESIAN_POINT('Ctrl Pts',(77.7353213865851,78.5958790582346,197.758333333333));
#32934=CARTESIAN_POINT('Ctrl Pts',(78.3731842446541,79.2640589050045,197.816666666667));
#32935=CARTESIAN_POINT('Ctrl Pts',(79.011047102723,79.9322387517744,197.875));
#32936=CARTESIAN_POINT('Ctrl Pts',(78.7513178101579,80.8187341143776,197.933333333333));
#32937=CARTESIAN_POINT('Ctrl Pts',(78.4915885175929,81.7052294769808,197.991666666667));
#32938=CARTESIAN_POINT('Ctrl Pts',(77.5939963669589,81.9235449928141,198.05));
#32939=CARTESIAN_POINT('Ctrl Pts',(77.2364435356502,82.0105102484145,198.073236888244));
#32940=CARTESIAN_POINT('Ctrl Pts',(76.8768229089103,81.9325359726461,198.1));
#32941=CARTESIAN_POINT('Origin',(76.882500972401,78.9982710885302,211.809374999522));
#32942=CARTESIAN_POINT('Origin',(76.882500972401,78.9982710885302,197.809374999522));
#32943=CARTESIAN_POINT('',(76.8377292359511,78.8141945740679,198.006249999044));
#32944=CARTESIAN_POINT('Origin',(77.2158628014545,80.368869783439,198.006249999044));
#32945=CARTESIAN_POINT('Origin',(77.215862801455,80.368869783441,211.6));
#32946=CARTESIAN_POINT('Origin',(77.2158628014545,80.368869783439,198.006249999044));
#32947=CARTESIAN_POINT('Origin',(77.215862801455,80.368869783441,198.1));
#32948=CARTESIAN_POINT('Origin',(77.215862801455,80.368869783441,211.6));
#32949=CARTESIAN_POINT('',(77.6885297583348,82.3122137951574,212.));
#32950=CARTESIAN_POINT('',(77.5939963669588,81.9235449928141,211.6));
#32951=CARTESIAN_POINT('Origin',(77.215862801455,80.368869783441,212.));
#32952=CARTESIAN_POINT('Origin',(77.215862801455,80.368869783441,197.7));
#32953=CARTESIAN_POINT('',(76.7431958445752,78.4255257717246,197.7));
#32954=CARTESIAN_POINT('',(76.7431958445752,78.4255257717246,197.7));
#32955=CARTESIAN_POINT('Origin',(77.215862801455,80.368869783441,197.7));
#32956=CARTESIAN_POINT('Origin',(77.215862801455,80.368869783441,198.1));
#32957=CARTESIAN_POINT('',(78.0666633238387,83.8668890045305,197.7));
#32958=CARTESIAN_POINT('',(78.1611967152146,84.2555578068738,198.1));
#32959=CARTESIAN_POINT('Origin',(77.215862801455,80.368869783441,197.7));
#32960=CARTESIAN_POINT('Origin',(77.215862801455,80.368869783441,212.));
#32961=CARTESIAN_POINT('',(76.2705288876953,76.4821817600082,211.6));
#32962=CARTESIAN_POINT('Origin',(77.215862801455,80.368869783441,211.6));
#32963=CARTESIAN_POINT('',(76.3650622790713,76.8708505623514,212.));
#32964=CARTESIAN_POINT('',(76.3650622790713,76.8708505623514,212.));
#32965=CARTESIAN_POINT('Origin',(77.215862801455,80.368869783441,212.));
#32966=CARTESIAN_POINT('Origin',(77.215862801455,80.368869783441,212.));
#32967=CARTESIAN_POINT('',(76.2705288876953,76.4821817600082,212.));
#32968=CARTESIAN_POINT('Origin',(77.215862801455,80.368869783441,197.7));
#32969=CARTESIAN_POINT('Origin',(77.215862801455,80.368869783441,212.));
#32970=CARTESIAN_POINT('Origin',(77.215862801455,80.368869783441,212.));
#32971=CARTESIAN_POINT('',(0.,0.,0.));
#32972=CARTESIAN_POINT('Origin',(7.2492530515395,16.403587196458,205.));
#32973=CARTESIAN_POINT('',(8.18272201375405,19.4755763502051,205.));
#32974=CARTESIAN_POINT('Origin',(10.0893624969369,19.4755763502051,205.));
#32975=CARTESIAN_POINT('',(13.0097794346237,24.6967371281661,205.));
#32976=CARTESIAN_POINT('',(6.22126690664867,17.3539789503745,205.));
#32977=CARTESIAN_POINT('Origin',(14.0377655795145,23.7463453742496,205.));
#32978=CARTESIAN_POINT('Origin',(41.0259406693811,-14.8235704322271,205.));
#32979=CARTESIAN_POINT('',(41.0434612989213,-14.8397685706175,206.399796645178));
#32980=CARTESIAN_POINT('',(41.0434612989212,-14.8397685706175,203.600203354821));
#32981=CARTESIAN_POINT('',(41.0434612989212,-14.8397685706175,197.5));
#32982=CARTESIAN_POINT('',(39.9979545244903,-13.8731786783106,205.));
#32983=CARTESIAN_POINT('Origin',(41.0259406693811,-14.8235704322271,205.));
#32984=CARTESIAN_POINT('Origin',(41.0259406693811,-14.8235704322271,205.));
#32985=CARTESIAN_POINT('Origin',(41.0259406693811,-14.8235704322271,205.));
#32986=CARTESIAN_POINT('Origin',(41.0109651979399,-14.8397685706176,205.));
#32987=CARTESIAN_POINT('',(46.7864670524653,-6.53042050051894,205.));
#32988=CARTESIAN_POINT('',(39.9979545244903,-13.8731786783106,205.));
#32989=CARTESIAN_POINT('Origin',(47.8144531973562,-7.48081225443545,205.));
#32990=CARTESIAN_POINT('Origin',(-13.7460461167398,28.868260502022,212.5));
#32991=CARTESIAN_POINT('',(-81.5490276261588,28.8682605020227,201.188219076791));
#32992=CARTESIAN_POINT('',(-81.1900532671845,28.8682605020226,201.393647762688));
#32993=CARTESIAN_POINT('',(-81.5490276261588,28.8682605020227,201.188219076791));
#32994=CARTESIAN_POINT('',(-81.5490276261588,28.8682605020227,201.726680615253));
#32995=CARTESIAN_POINT('',(-81.5490276261588,28.8682605020227,201.726680615253));
#32996=CARTESIAN_POINT('',(-84.6900532671845,28.8682605020227,201.726680615253));
#32997=CARTESIAN_POINT('',(-84.6900532671845,28.8682605020227,201.726680615253));
#32998=CARTESIAN_POINT('',(-84.6900532671845,28.8682605020227,202.040783179355));
#32999=CARTESIAN_POINT('',(-84.6900532671845,28.8682605020227,202.040783179355));
#33000=CARTESIAN_POINT('',(-81.1900532671845,28.8682605020226,202.040783179355));
#33001=CARTESIAN_POINT('',(-81.1900532671845,28.8682605020226,202.040783179355));
#33002=CARTESIAN_POINT('',(-81.1900532671845,28.8682605020226,201.393647762688));
#33003=CARTESIAN_POINT('Origin',(-81.5490276261588,28.8682605020227,201.726680615253));
#33004=CARTESIAN_POINT('',(-81.5490276261588,29.0682605020227,201.726680615253));
#33005=CARTESIAN_POINT('',(-81.5490276261588,29.0682605020227,201.188219076791));
#33006=CARTESIAN_POINT('',(-81.5490276261588,29.0682605020227,201.726680615253));
#33007=CARTESIAN_POINT('',(-81.5490276261588,28.8682605020227,201.726680615253));
#33008=CARTESIAN_POINT('',(-81.5490276261588,28.8682605020227,201.188219076791));
#33009=CARTESIAN_POINT('Origin',(-84.6900532671845,28.8682605020227,201.726680615253));
#33010=CARTESIAN_POINT('',(-84.6900532671845,29.0682605020227,201.726680615253));
#33011=CARTESIAN_POINT('',(-84.6900532671845,29.0682605020227,201.726680615253));
#33012=CARTESIAN_POINT('',(-84.6900532671845,28.8682605020227,201.726680615253));
#33013=CARTESIAN_POINT('Origin',(-84.6900532671845,28.8682605020227,202.040783179355));
#33014=CARTESIAN_POINT('',(-84.6900532671845,29.0682605020227,202.040783179355));
#33015=CARTESIAN_POINT('',(-84.6900532671845,29.0682605020227,202.040783179355));
#33016=CARTESIAN_POINT('',(-84.6900532671845,28.8682605020227,202.040783179355));
#33017=CARTESIAN_POINT('Origin',(-81.1900532671845,28.8682605020226,202.040783179355));
#33018=CARTESIAN_POINT('',(-81.1900532671845,29.0682605020227,202.040783179355));
#33019=CARTESIAN_POINT('',(-81.1900532671845,29.0682605020227,202.040783179355));
#33020=CARTESIAN_POINT('',(-81.1900532671845,28.8682605020226,202.040783179355));
#33021=CARTESIAN_POINT('Origin',(-81.1900532671845,28.8682605020226,201.393647762688));
#33022=CARTESIAN_POINT('',(-81.1900532671845,29.0682605020227,201.393647762688));
#33023=CARTESIAN_POINT('',(-81.1900532671845,29.0682605020227,201.393647762688));
#33024=CARTESIAN_POINT('',(-81.1900532671845,28.8682605020226,201.393647762688));
#33025=CARTESIAN_POINT('Origin',(-81.5490276261588,28.8682605020227,201.188219076791));
#33026=CARTESIAN_POINT('',(-81.5490276261588,29.0682605020227,201.188219076791));
#33027=CARTESIAN_POINT('Origin',(-81.6887029333228,28.8682605020227,204.026105282754));
#33028=CARTESIAN_POINT('',(-81.4592840364153,28.8682605020227,204.601981096022));
#33029=CARTESIAN_POINT('',(-82.2669763441075,28.8682605020227,203.790783179355));
#33030=CARTESIAN_POINT('Ctrl Pts',(-81.4592840364153,28.8682605020227,204.601981096022));
#33031=CARTESIAN_POINT('Ctrl Pts',(-81.4599708546575,28.8682605020227,204.574603393385));
#33032=CARTESIAN_POINT('Ctrl Pts',(-81.4613196522816,28.8682605020227,204.520838105856));
#33033=CARTESIAN_POINT('Ctrl Pts',(-81.471536117869,28.8682605020227,204.442066315421));
#33034=CARTESIAN_POINT('Ctrl Pts',(-81.4870242844412,28.8682605020227,204.366402575227));
#33035=CARTESIAN_POINT('Ctrl Pts',(-81.5116228732431,28.8682605020227,204.294975855603));
#33036=CARTESIAN_POINT('Ctrl Pts',(-81.5406873285984,28.8682605020227,204.226239456265));
#33037=CARTESIAN_POINT('Ctrl Pts',(-81.5776105868505,28.8682605020227,204.161660790704));
#33038=CARTESIAN_POINT('Ctrl Pts',(-81.6205162333266,28.8682605020227,204.100167655303));
#33039=CARTESIAN_POINT('Ctrl Pts',(-81.6702670801791,28.8682605020227,204.042771493033));
#33040=CARTESIAN_POINT('Ctrl Pts',(-81.7261657529711,28.8682605020227,203.990350529552));
#33041=CARTESIAN_POINT('Ctrl Pts',(-81.7877699492256,28.8682605020227,203.943644208757));
#33042=CARTESIAN_POINT('Ctrl Pts',(-81.8546361678019,28.8682605020226,203.903103127741));
#33043=CARTESIAN_POINT('Ctrl Pts',(-81.9264899768362,28.8682605020227,203.867682009478));
#33044=CARTESIAN_POINT('Ctrl Pts',(-82.004046772439,28.8682605020227,203.838929655973));
#33045=CARTESIAN_POINT('Ctrl Pts',(-82.087013622034,28.8682605020227,203.816955559262));
#33046=CARTESIAN_POINT('Ctrl Pts',(-82.1750352431015,28.8682605020227,203.799568977673));
#33047=CARTESIAN_POINT('Ctrl Pts',(-82.2358202943267,28.8682605020227,203.793760419858));
#33048=CARTESIAN_POINT('Ctrl Pts',(-82.2669763441075,28.8682605020227,203.790783179355));
#33049=CARTESIAN_POINT('',(-82.1688192928255,28.8682605020227,205.361295999868));
#33050=CARTESIAN_POINT('Ctrl Pts',(-82.1688192928255,28.8682605020227,205.361295999868));
#33051=CARTESIAN_POINT('Ctrl Pts',(-82.1449378944147,28.8682605020227,205.360660257568));
#33052=CARTESIAN_POINT('Ctrl Pts',(-82.0978722440534,28.8682605020227,205.359407331577));
#33053=CARTESIAN_POINT('Ctrl Pts',(-82.0288664850348,28.8682605020227,205.348349634083));
#33054=CARTESIAN_POINT('Ctrl Pts',(-81.962301671219,28.8682605020227,205.331639127989));
#33055=CARTESIAN_POINT('Ctrl Pts',(-81.8979730521012,28.8682605020226,205.307693869941));
#33056=CARTESIAN_POINT('Ctrl Pts',(-81.836527400035,28.8682605020227,205.276087129855));
#33057=CARTESIAN_POINT('Ctrl Pts',(-81.7778899198314,28.8682605020226,205.237613749938));
#33058=CARTESIAN_POINT('Ctrl Pts',(-81.7212009546313,28.8682605020227,205.19322368652));
#33059=CARTESIAN_POINT('Ctrl Pts',(-81.6680476565732,28.8682605020226,205.141872417189));
#33060=CARTESIAN_POINT('Ctrl Pts',(-81.6193664510908,28.8682605020227,205.085460897382));
#33061=CARTESIAN_POINT('Ctrl Pts',(-81.5762423656764,28.8682605020226,205.025866647797));
#33062=CARTESIAN_POINT('Ctrl Pts',(-81.5402032548776,28.8682605020227,204.962816543537));
#33063=CARTESIAN_POINT('Ctrl Pts',(-81.5106597576971,28.8682605020226,204.896576421361));
#33064=CARTESIAN_POINT('Ctrl Pts',(-81.4874843765008,28.8682605020227,204.827330951953));
#33065=CARTESIAN_POINT('Ctrl Pts',(-81.4714257970777,28.8682605020227,204.754946206831));
#33066=CARTESIAN_POINT('Ctrl Pts',(-81.461343313131,28.8682605020227,204.679622190548));
#33067=CARTESIAN_POINT('Ctrl Pts',(-81.4599791412227,28.8682605020227,204.628188694857));
#33068=CARTESIAN_POINT('Ctrl Pts',(-81.4592840364153,28.8682605020227,204.601981096022));
#33069=CARTESIAN_POINT('',(-83.2415356389794,28.8682605020227,204.699437025509));
#33070=CARTESIAN_POINT('Ctrl Pts',(-83.2415356389794,28.8682605020227,204.699437025509));
#33071=CARTESIAN_POINT('Ctrl Pts',(-83.2070373324308,28.8682605020227,204.732484912317));
#33072=CARTESIAN_POINT('Ctrl Pts',(-83.1407731458266,28.8682605020227,204.795963139436));
#33073=CARTESIAN_POINT('Ctrl Pts',(-83.0440301856925,28.8682605020227,204.885745716245));
#33074=CARTESIAN_POINT('Ctrl Pts',(-82.9542806449404,28.8682605020227,204.966384704557));
#33075=CARTESIAN_POINT('Ctrl Pts',(-82.8716940964959,28.8682605020227,205.038402097329));
#33076=CARTESIAN_POINT('Ctrl Pts',(-82.7950625287004,28.8682605020227,205.100235602695));
#33077=CARTESIAN_POINT('Ctrl Pts',(-82.7268678251126,28.8682605020227,205.155107834643));
#33078=CARTESIAN_POINT('Ctrl Pts',(-82.6641133748048,28.8682605020227,205.199073425625));
#33079=CARTESIAN_POINT('Ctrl Pts',(-82.5913727608922,28.8682605020227,205.246788821312));
#33080=CARTESIAN_POINT('Ctrl Pts',(-82.5025604437182,28.8682605020227,205.293002802711));
#33081=CARTESIAN_POINT('Ctrl Pts',(-82.3940267544571,28.8682605020227,205.332715158751));
#33082=CARTESIAN_POINT('Ctrl Pts',(-82.2822995017811,28.8682605020226,205.3569300072));
#33083=CARTESIAN_POINT('Ctrl Pts',(-82.2067974647339,28.8682605020227,205.359834842706));
#33084=CARTESIAN_POINT('Ctrl Pts',(-82.1688192928255,28.8682605020227,205.361295999868));
#33085=CARTESIAN_POINT('',(-84.6900532671845,28.8682605020227,203.342065230637));
#33086=CARTESIAN_POINT('',(-84.6900532671845,28.8682605020227,203.342065230637));
#33087=CARTESIAN_POINT('',(-84.6900532671844,28.8682605020227,205.720270358842));
#33088=CARTESIAN_POINT('',(-84.6900532671844,28.8682605020227,205.720270358842));
#33089=CARTESIAN_POINT('',(-84.33107890821,28.8682605020227,205.720270358842));
#33090=CARTESIAN_POINT('',(-84.33107890821,28.8682605020227,205.720270358842));
#33091=CARTESIAN_POINT('',(-84.33107890821,28.8682605020227,204.091564429355));
#33092=CARTESIAN_POINT('',(-84.33107890821,28.8682605020227,204.091564429355));
#33093=CARTESIAN_POINT('',(-83.396483555646,28.8682605020227,204.96726555115));
#33094=CARTESIAN_POINT('',(-83.396483555646,28.8682605020227,204.96726555115));
#33095=CARTESIAN_POINT('',(-82.1407744210305,28.8682605020227,205.67539856397));
#33096=CARTESIAN_POINT('Ctrl Pts',(-82.1407744210305,28.8682605020227,205.67539856397));
#33097=CARTESIAN_POINT('Ctrl Pts',(-82.1895222346161,28.8682605020227,205.673705274502));
#33098=CARTESIAN_POINT('Ctrl Pts',(-82.2861624066765,28.8682605020227,205.670348410399));
#33099=CARTESIAN_POINT('Ctrl Pts',(-82.4281775770736,28.8682605020227,205.64163442389));
#33100=CARTESIAN_POINT('Ctrl Pts',(-82.5657698252851,28.8682605020227,205.596786428274));
#33101=CARTESIAN_POINT('Ctrl Pts',(-82.6765109016597,28.8682605020227,205.542793856741));
#33102=CARTESIAN_POINT('Ctrl Pts',(-82.7657359477164,28.8682605020227,205.488310702079));
#33103=CARTESIAN_POINT('Ctrl Pts',(-82.8392357134513,28.8682605020227,205.439262575613));
#33104=CARTESIAN_POINT('Ctrl Pts',(-82.9183543749108,28.8682605020227,205.381517084423));
#33105=CARTESIAN_POINT('Ctrl Pts',(-83.0034121639627,28.8682605020227,205.315567580555));
#33106=CARTESIAN_POINT('Ctrl Pts',(-83.0932951769942,28.8682605020227,205.240278319977));
#33107=CARTESIAN_POINT('Ctrl Pts',(-83.1898372690957,28.8682605020227,205.157605307559));
#33108=CARTESIAN_POINT('Ctrl Pts',(-83.2912533102384,28.8682605020227,205.065413484233));
#33109=CARTESIAN_POINT('Ctrl Pts',(-83.3605669592593,28.8682605020227,205.000764852468));
#33110=CARTESIAN_POINT('Ctrl Pts',(-83.396483555646,28.8682605020227,204.96726555115));
#33111=CARTESIAN_POINT('',(-81.1003096774409,28.8682605020226,204.618106897304));
#33112=CARTESIAN_POINT('Ctrl Pts',(-81.1003096774409,28.8682605020226,204.618106897304));
#33113=CARTESIAN_POINT('Ctrl Pts',(-81.1012008428613,28.8682605020226,204.656487672198));
#33114=CARTESIAN_POINT('Ctrl Pts',(-81.1029519510787,28.8682605020226,204.731904523843));
#33115=CARTESIAN_POINT('Ctrl Pts',(-81.1182161233739,28.8682605020226,204.841928331133));
#33116=CARTESIAN_POINT('Ctrl Pts',(-81.1416071069158,28.8682605020227,204.946917430261));
#33117=CARTESIAN_POINT('Ctrl Pts',(-81.1762688598019,28.8682605020226,205.045681980795));
#33118=CARTESIAN_POINT('Ctrl Pts',(-81.219761777561,28.8682605020227,205.139235584572));
#33119=CARTESIAN_POINT('Ctrl Pts',(-81.2738509190422,28.8682605020226,205.226419892733));
#33120=CARTESIAN_POINT('Ctrl Pts',(-81.3359769680758,28.8682605020227,205.309343112776));
#33121=CARTESIAN_POINT('Ctrl Pts',(-81.409257689452,28.8682605020227,205.383935517473));
#33122=CARTESIAN_POINT('Ctrl Pts',(-81.4874484042645,28.8682605020227,205.452457639886));
#33123=CARTESIAN_POINT('Ctrl Pts',(-81.5709554302159,28.8682605020226,205.51151956653));
#33124=CARTESIAN_POINT('Ctrl Pts',(-81.6573042663379,28.8682605020226,205.562384162401));
#33125=CARTESIAN_POINT('Ctrl Pts',(-81.7471694226447,28.8682605020227,205.604015245344));
#33126=CARTESIAN_POINT('Ctrl Pts',(-81.8408435437684,28.8682605020227,205.635573457601));
#33127=CARTESIAN_POINT('Ctrl Pts',(-81.937428543862,28.8682605020227,205.658955068432));
#33128=CARTESIAN_POINT('Ctrl Pts',(-82.0380390792887,28.8682605020227,205.672321260714));
#33129=CARTESIAN_POINT('Ctrl Pts',(-82.1061475940205,28.8682605020227,205.6743613625));
#33130=CARTESIAN_POINT('Ctrl Pts',(-82.1407744210305,28.8682605020227,205.67539856397));
#33131=CARTESIAN_POINT('',(-82.2669763441076,28.8682605020227,203.476680615253));
#33132=CARTESIAN_POINT('Ctrl Pts',(-82.2669763441076,28.8682605020227,203.476680615253));
#33133=CARTESIAN_POINT('Ctrl Pts',(-82.2253054563398,28.8682605020227,203.47872776826));
#33134=CARTESIAN_POINT('Ctrl Pts',(-82.1434649417649,28.8682605020227,203.482748322286));
#33135=CARTESIAN_POINT('Ctrl Pts',(-82.0241410353658,28.8682605020227,203.501576611548));
#33136=CARTESIAN_POINT('Ctrl Pts',(-81.9100862366409,28.8682605020227,203.528517488753));
#33137=CARTESIAN_POINT('Ctrl Pts',(-81.8022163226713,28.8682605020227,203.566608942768));
#33138=CARTESIAN_POINT('Ctrl Pts',(-81.6995775154409,28.8682605020226,203.613915220538));
#33139=CARTESIAN_POINT('Ctrl Pts',(-81.6025774997497,28.8682605020227,203.670645247919));
#33140=CARTESIAN_POINT('Ctrl Pts',(-81.511586311035,28.8682605020227,203.737839098432));
#33141=CARTESIAN_POINT('Ctrl Pts',(-81.4274474677396,28.8682605020226,203.814045832477));
#33142=CARTESIAN_POINT('Ctrl Pts',(-81.3502598969403,28.8682605020227,203.896814471532));
#33143=CARTESIAN_POINT('Ctrl Pts',(-81.2836046541341,28.8682605020227,203.986120411003));
#33144=CARTESIAN_POINT('Ctrl Pts',(-81.2272869827721,28.8682605020226,204.07996543829));
#33145=CARTESIAN_POINT('Ctrl Pts',(-81.1802057409483,28.8682605020227,204.178064837255));
#33146=CARTESIAN_POINT('Ctrl Pts',(-81.1448658950257,28.8682605020226,204.281525400815));
#33147=CARTESIAN_POINT('Ctrl Pts',(-81.1186442554211,28.8682605020226,204.389408258654));
#33148=CARTESIAN_POINT('Ctrl Pts',(-81.1028679096996,28.8682605020227,204.502187395063));
#33149=CARTESIAN_POINT('Ctrl Pts',(-81.1011721240953,28.8682605020226,204.57902741711));
#33150=CARTESIAN_POINT('Ctrl Pts',(-81.1003096774409,28.8682605020226,204.618106897304));
#33151=CARTESIAN_POINT('',(-82.2669763441075,28.8682605020227,203.790783179355));
#33152=CARTESIAN_POINT('Ctrl Pts',(-82.1688192928255,28.8682605020227,205.361295999868));
#33153=CARTESIAN_POINT('Ctrl Pts',(-82.1688192928255,29.1082605020227,205.361295999868));
#33154=CARTESIAN_POINT('Ctrl Pts',(-82.1449378944147,28.8682605020227,205.360660257568));
#33155=CARTESIAN_POINT('Ctrl Pts',(-82.1449378944147,29.1082605020227,205.360660257568));
#33156=CARTESIAN_POINT('Ctrl Pts',(-82.0978722440534,28.8682605020227,205.359407331577));
#33157=CARTESIAN_POINT('Ctrl Pts',(-82.0978722440534,29.1082605020227,205.359407331577));
#33158=CARTESIAN_POINT('Ctrl Pts',(-82.0288664850348,28.8682605020227,205.348349634083));
#33159=CARTESIAN_POINT('Ctrl Pts',(-82.0288664850348,29.1082605020227,205.348349634083));
#33160=CARTESIAN_POINT('Ctrl Pts',(-81.962301671219,28.8682605020227,205.331639127989));
#33161=CARTESIAN_POINT('Ctrl Pts',(-81.962301671219,29.1082605020227,205.331639127989));
#33162=CARTESIAN_POINT('Ctrl Pts',(-81.8979730521012,28.8682605020226,205.307693869941));
#33163=CARTESIAN_POINT('Ctrl Pts',(-81.8979730521012,29.1082605020226,205.307693869941));
#33164=CARTESIAN_POINT('Ctrl Pts',(-81.836527400035,28.8682605020227,205.276087129855));
#33165=CARTESIAN_POINT('Ctrl Pts',(-81.836527400035,29.1082605020227,205.276087129855));
#33166=CARTESIAN_POINT('Ctrl Pts',(-81.7778899198314,28.8682605020226,205.237613749938));
#33167=CARTESIAN_POINT('Ctrl Pts',(-81.7778899198314,29.1082605020226,205.237613749938));
#33168=CARTESIAN_POINT('Ctrl Pts',(-81.7212009546313,28.8682605020227,205.19322368652));
#33169=CARTESIAN_POINT('Ctrl Pts',(-81.7212009546313,29.1082605020227,205.19322368652));
#33170=CARTESIAN_POINT('Ctrl Pts',(-81.6680476565732,28.8682605020226,205.141872417189));
#33171=CARTESIAN_POINT('Ctrl Pts',(-81.6680476565732,29.1082605020226,205.141872417189));
#33172=CARTESIAN_POINT('Ctrl Pts',(-81.6193664510908,28.8682605020227,205.085460897382));
#33173=CARTESIAN_POINT('Ctrl Pts',(-81.6193664510908,29.1082605020227,205.085460897382));
#33174=CARTESIAN_POINT('Ctrl Pts',(-81.5762423656764,28.8682605020226,205.025866647797));
#33175=CARTESIAN_POINT('Ctrl Pts',(-81.5762423656764,29.1082605020226,205.025866647797));
#33176=CARTESIAN_POINT('Ctrl Pts',(-81.5402032548776,28.8682605020227,204.962816543537));
#33177=CARTESIAN_POINT('Ctrl Pts',(-81.5402032548776,29.1082605020227,204.962816543537));
#33178=CARTESIAN_POINT('Ctrl Pts',(-81.5106597576971,28.8682605020226,204.896576421361));
#33179=CARTESIAN_POINT('Ctrl Pts',(-81.5106597576971,29.1082605020226,204.896576421361));
#33180=CARTESIAN_POINT('Ctrl Pts',(-81.4874843765008,28.8682605020226,204.827330951953));
#33181=CARTESIAN_POINT('Ctrl Pts',(-81.4874843765008,29.1082605020226,204.827330951953));
#33182=CARTESIAN_POINT('Ctrl Pts',(-81.4714257970777,28.8682605020226,204.754946206831));
#33183=CARTESIAN_POINT('Ctrl Pts',(-81.4714257970777,29.1082605020226,204.754946206831));
#33184=CARTESIAN_POINT('Ctrl Pts',(-81.461343313131,28.8682605020226,204.679622190548));
#33185=CARTESIAN_POINT('Ctrl Pts',(-81.461343313131,29.1082605020226,204.679622190548));
#33186=CARTESIAN_POINT('Ctrl Pts',(-81.4599791412227,28.8682605020226,204.628188694857));
#33187=CARTESIAN_POINT('Ctrl Pts',(-81.4599791412227,29.1082605020226,204.628188694857));
#33188=CARTESIAN_POINT('Ctrl Pts',(-81.4592840364153,28.8682605020226,204.601981096022));
#33189=CARTESIAN_POINT('Ctrl Pts',(-81.4592840364153,29.1082605020226,204.601981096022));
#33190=CARTESIAN_POINT('',(-82.1688192928255,29.0682605020227,205.361295999868));
#33191=CARTESIAN_POINT('',(-81.4592840364153,29.0682605020227,204.601981096022));
#33192=CARTESIAN_POINT('Ctrl Pts',(-82.1688192928255,29.0682605020227,205.361295999868));
#33193=CARTESIAN_POINT('Ctrl Pts',(-82.1449378944147,29.0682605020227,205.360660257568));
#33194=CARTESIAN_POINT('Ctrl Pts',(-82.0978722440534,29.0682605020227,205.359407331577));
#33195=CARTESIAN_POINT('Ctrl Pts',(-82.0288664850348,29.0682605020227,205.348349634083));
#33196=CARTESIAN_POINT('Ctrl Pts',(-81.962301671219,29.0682605020227,205.331639127989));
#33197=CARTESIAN_POINT('Ctrl Pts',(-81.8979730521012,29.0682605020227,205.307693869941));
#33198=CARTESIAN_POINT('Ctrl Pts',(-81.836527400035,29.0682605020227,205.276087129855));
#33199=CARTESIAN_POINT('Ctrl Pts',(-81.7778899198314,29.0682605020227,205.237613749938));
#33200=CARTESIAN_POINT('Ctrl Pts',(-81.7212009546313,29.0682605020227,205.19322368652));
#33201=CARTESIAN_POINT('Ctrl Pts',(-81.6680476565732,29.0682605020227,205.141872417189));
#33202=CARTESIAN_POINT('Ctrl Pts',(-81.6193664510908,29.0682605020227,205.085460897382));
#33203=CARTESIAN_POINT('Ctrl Pts',(-81.5762423656764,29.0682605020227,205.025866647797));
#33204=CARTESIAN_POINT('Ctrl Pts',(-81.5402032548776,29.0682605020227,204.962816543537));
#33205=CARTESIAN_POINT('Ctrl Pts',(-81.5106597576971,29.0682605020226,204.896576421361));
#33206=CARTESIAN_POINT('Ctrl Pts',(-81.4874843765008,29.0682605020227,204.827330951953));
#33207=CARTESIAN_POINT('Ctrl Pts',(-81.4714257970777,29.0682605020227,204.754946206831));
#33208=CARTESIAN_POINT('Ctrl Pts',(-81.461343313131,29.0682605020227,204.679622190548));
#33209=CARTESIAN_POINT('Ctrl Pts',(-81.4599791412227,29.0682605020227,204.628188694857));
#33210=CARTESIAN_POINT('Ctrl Pts',(-81.4592840364153,29.0682605020227,204.601981096022));
#33211=CARTESIAN_POINT('',(-82.1688192928255,28.8682605020227,205.361295999868));
#33212=CARTESIAN_POINT('',(-81.4592840364153,28.8682605020227,204.601981096022));
#33213=CARTESIAN_POINT('Ctrl Pts',(-83.2415356389794,28.8682605020227,204.699437025509));
#33214=CARTESIAN_POINT('Ctrl Pts',(-83.2415356389794,29.1082605020227,204.699437025509));
#33215=CARTESIAN_POINT('Ctrl Pts',(-83.2070373324308,28.8682605020227,204.732484912317));
#33216=CARTESIAN_POINT('Ctrl Pts',(-83.2070373324308,29.1082605020227,204.732484912317));
#33217=CARTESIAN_POINT('Ctrl Pts',(-83.1407731458266,28.8682605020227,204.795963139436));
#33218=CARTESIAN_POINT('Ctrl Pts',(-83.1407731458266,29.1082605020227,204.795963139436));
#33219=CARTESIAN_POINT('Ctrl Pts',(-83.0440301856925,28.8682605020227,204.885745716245));
#33220=CARTESIAN_POINT('Ctrl Pts',(-83.0440301856925,29.1082605020227,204.885745716245));
#33221=CARTESIAN_POINT('Ctrl Pts',(-82.9542806449404,28.8682605020227,204.966384704557));
#33222=CARTESIAN_POINT('Ctrl Pts',(-82.9542806449404,29.1082605020227,204.966384704557));
#33223=CARTESIAN_POINT('Ctrl Pts',(-82.8716940964959,28.8682605020227,205.038402097329));
#33224=CARTESIAN_POINT('Ctrl Pts',(-82.8716940964959,29.1082605020227,205.038402097329));
#33225=CARTESIAN_POINT('Ctrl Pts',(-82.7950625287004,28.8682605020227,205.100235602695));
#33226=CARTESIAN_POINT('Ctrl Pts',(-82.7950625287004,29.1082605020227,205.100235602695));
#33227=CARTESIAN_POINT('Ctrl Pts',(-82.7268678251126,28.8682605020227,205.155107834643));
#33228=CARTESIAN_POINT('Ctrl Pts',(-82.7268678251126,29.1082605020227,205.155107834643));
#33229=CARTESIAN_POINT('Ctrl Pts',(-82.6641133748048,28.8682605020227,205.199073425625));
#33230=CARTESIAN_POINT('Ctrl Pts',(-82.6641133748048,29.1082605020227,205.199073425625));
#33231=CARTESIAN_POINT('Ctrl Pts',(-82.5913727608922,28.8682605020227,205.246788821312));
#33232=CARTESIAN_POINT('Ctrl Pts',(-82.5913727608922,29.1082605020227,205.246788821312));
#33233=CARTESIAN_POINT('Ctrl Pts',(-82.5025604437182,28.8682605020227,205.293002802711));
#33234=CARTESIAN_POINT('Ctrl Pts',(-82.5025604437182,29.1082605020227,205.293002802711));
#33235=CARTESIAN_POINT('Ctrl Pts',(-82.3940267544571,28.8682605020227,205.332715158751));
#33236=CARTESIAN_POINT('Ctrl Pts',(-82.3940267544571,29.1082605020227,205.332715158751));
#33237=CARTESIAN_POINT('Ctrl Pts',(-82.2822995017811,28.8682605020226,205.3569300072));
#33238=CARTESIAN_POINT('Ctrl Pts',(-82.2822995017811,29.1082605020226,205.3569300072));
#33239=CARTESIAN_POINT('Ctrl Pts',(-82.2067974647339,28.8682605020227,205.359834842706));
#33240=CARTESIAN_POINT('Ctrl Pts',(-82.2067974647339,29.1082605020227,205.359834842706));
#33241=CARTESIAN_POINT('Ctrl Pts',(-82.1688192928255,28.8682605020227,205.361295999868));
#33242=CARTESIAN_POINT('Ctrl Pts',(-82.1688192928255,29.1082605020227,205.361295999868));
#33243=CARTESIAN_POINT('',(-83.2415356389794,29.0682605020227,204.699437025509));
#33244=CARTESIAN_POINT('Ctrl Pts',(-83.2415356389794,29.0682605020227,204.699437025509));
#33245=CARTESIAN_POINT('Ctrl Pts',(-83.2070373324308,29.0682605020227,204.732484912317));
#33246=CARTESIAN_POINT('Ctrl Pts',(-83.1407731458266,29.0682605020227,204.795963139436));
#33247=CARTESIAN_POINT('Ctrl Pts',(-83.0440301856925,29.0682605020227,204.885745716245));
#33248=CARTESIAN_POINT('Ctrl Pts',(-82.9542806449404,29.0682605020227,204.966384704557));
#33249=CARTESIAN_POINT('Ctrl Pts',(-82.8716940964959,29.0682605020227,205.038402097329));
#33250=CARTESIAN_POINT('Ctrl Pts',(-82.7950625287004,29.0682605020227,205.100235602695));
#33251=CARTESIAN_POINT('Ctrl Pts',(-82.7268678251126,29.0682605020227,205.155107834643));
#33252=CARTESIAN_POINT('Ctrl Pts',(-82.6641133748048,29.0682605020227,205.199073425625));
#33253=CARTESIAN_POINT('Ctrl Pts',(-82.5913727608922,29.0682605020227,205.246788821312));
#33254=CARTESIAN_POINT('Ctrl Pts',(-82.5025604437182,29.0682605020227,205.293002802711));
#33255=CARTESIAN_POINT('Ctrl Pts',(-82.3940267544571,29.0682605020227,205.332715158751));
#33256=CARTESIAN_POINT('Ctrl Pts',(-82.2822995017811,29.0682605020227,205.3569300072));
#33257=CARTESIAN_POINT('Ctrl Pts',(-82.2067974647339,29.0682605020227,205.359834842706));
#33258=CARTESIAN_POINT('Ctrl Pts',(-82.1688192928255,29.0682605020227,205.361295999868));
#33259=CARTESIAN_POINT('',(-83.2415356389794,28.8682605020227,204.699437025509));
#33260=CARTESIAN_POINT('Origin',(-84.6900532671845,28.8682605020227,203.342065230637));
#33261=CARTESIAN_POINT('',(-84.6900532671845,29.0682605020227,203.342065230637));
#33262=CARTESIAN_POINT('',(-84.6900532671845,29.0682605020227,203.342065230637));
#33263=CARTESIAN_POINT('',(-84.6900532671845,28.8682605020227,203.342065230637));
#33264=CARTESIAN_POINT('Origin',(-84.6900532671844,28.8682605020227,205.720270358842));
#33265=CARTESIAN_POINT('',(-84.6900532671844,29.0682605020227,205.720270358842));
#33266=CARTESIAN_POINT('',(-84.6900532671844,29.0682605020227,205.720270358842));
#33267=CARTESIAN_POINT('',(-84.6900532671844,28.8682605020227,205.720270358842));
#33268=CARTESIAN_POINT('Origin',(-84.33107890821,28.8682605020227,205.720270358842));
#33269=CARTESIAN_POINT('',(-84.33107890821,29.0682605020227,205.720270358842));
#33270=CARTESIAN_POINT('',(-84.33107890821,29.0682605020227,205.720270358842));
#33271=CARTESIAN_POINT('',(-84.33107890821,28.8682605020227,205.720270358842));
#33272=CARTESIAN_POINT('Origin',(-84.33107890821,28.8682605020227,204.091564429355));
#33273=CARTESIAN_POINT('',(-84.33107890821,29.0682605020227,204.091564429355));
#33274=CARTESIAN_POINT('',(-84.33107890821,29.0682605020227,204.091564429355));
#33275=CARTESIAN_POINT('',(-84.33107890821,28.8682605020227,204.091564429355));
#33276=CARTESIAN_POINT('Origin',(-83.396483555646,28.8682605020227,204.96726555115));
#33277=CARTESIAN_POINT('',(-83.396483555646,29.0682605020227,204.96726555115));
#33278=CARTESIAN_POINT('',(-83.396483555646,29.0682605020227,204.96726555115));
#33279=CARTESIAN_POINT('',(-83.396483555646,28.8682605020227,204.96726555115));
#33280=CARTESIAN_POINT('Ctrl Pts',(-82.1407744210305,28.8682605020227,205.67539856397));
#33281=CARTESIAN_POINT('Ctrl Pts',(-82.1407744210305,29.1082605020227,205.67539856397));
#33282=CARTESIAN_POINT('Ctrl Pts',(-82.1895222346161,28.8682605020227,205.673705274502));
#33283=CARTESIAN_POINT('Ctrl Pts',(-82.1895222346161,29.1082605020227,205.673705274502));
#33284=CARTESIAN_POINT('Ctrl Pts',(-82.2861624066765,28.8682605020227,205.670348410399));
#33285=CARTESIAN_POINT('Ctrl Pts',(-82.2861624066765,29.1082605020227,205.670348410399));
#33286=CARTESIAN_POINT('Ctrl Pts',(-82.4281775770736,28.8682605020227,205.64163442389));
#33287=CARTESIAN_POINT('Ctrl Pts',(-82.4281775770736,29.1082605020227,205.64163442389));
#33288=CARTESIAN_POINT('Ctrl Pts',(-82.5657698252851,28.8682605020227,205.596786428274));
#33289=CARTESIAN_POINT('Ctrl Pts',(-82.5657698252851,29.1082605020227,205.596786428274));
#33290=CARTESIAN_POINT('Ctrl Pts',(-82.6765109016597,28.8682605020227,205.542793856741));
#33291=CARTESIAN_POINT('Ctrl Pts',(-82.6765109016597,29.1082605020227,205.542793856741));
#33292=CARTESIAN_POINT('Ctrl Pts',(-82.7657359477164,28.8682605020227,205.488310702079));
#33293=CARTESIAN_POINT('Ctrl Pts',(-82.7657359477164,29.1082605020227,205.488310702079));
#33294=CARTESIAN_POINT('Ctrl Pts',(-82.8392357134513,28.8682605020227,205.439262575613));
#33295=CARTESIAN_POINT('Ctrl Pts',(-82.8392357134513,29.1082605020227,205.439262575613));
#33296=CARTESIAN_POINT('Ctrl Pts',(-82.9183543749108,28.8682605020227,205.381517084423));
#33297=CARTESIAN_POINT('Ctrl Pts',(-82.9183543749108,29.1082605020227,205.381517084423));
#33298=CARTESIAN_POINT('Ctrl Pts',(-83.0034121639627,28.8682605020227,205.315567580555));
#33299=CARTESIAN_POINT('Ctrl Pts',(-83.0034121639627,29.1082605020227,205.315567580555));
#33300=CARTESIAN_POINT('Ctrl Pts',(-83.0932951769942,28.8682605020227,205.240278319977));
#33301=CARTESIAN_POINT('Ctrl Pts',(-83.0932951769942,29.1082605020227,205.240278319977));
#33302=CARTESIAN_POINT('Ctrl Pts',(-83.1898372690957,28.8682605020227,205.157605307559));
#33303=CARTESIAN_POINT('Ctrl Pts',(-83.1898372690957,29.1082605020227,205.157605307559));
#33304=CARTESIAN_POINT('Ctrl Pts',(-83.2912533102384,28.8682605020227,205.065413484233));
#33305=CARTESIAN_POINT('Ctrl Pts',(-83.2912533102384,29.1082605020227,205.065413484233));
#33306=CARTESIAN_POINT('Ctrl Pts',(-83.3605669592593,28.8682605020227,205.000764852468));
#33307=CARTESIAN_POINT('Ctrl Pts',(-83.3605669592593,29.1082605020227,205.000764852468));
#33308=CARTESIAN_POINT('Ctrl Pts',(-83.396483555646,28.8682605020227,204.96726555115));
#33309=CARTESIAN_POINT('Ctrl Pts',(-83.396483555646,29.1082605020227,204.96726555115));
#33310=CARTESIAN_POINT('',(-82.1407744210305,29.0682605020227,205.67539856397));
#33311=CARTESIAN_POINT('Ctrl Pts',(-82.1407744210305,29.0682605020227,205.67539856397));
#33312=CARTESIAN_POINT('Ctrl Pts',(-82.1895222346161,29.0682605020227,205.673705274502));
#33313=CARTESIAN_POINT('Ctrl Pts',(-82.2861624066765,29.0682605020227,205.670348410399));
#33314=CARTESIAN_POINT('Ctrl Pts',(-82.4281775770736,29.0682605020227,205.64163442389));
#33315=CARTESIAN_POINT('Ctrl Pts',(-82.5657698252851,29.0682605020227,205.596786428274));
#33316=CARTESIAN_POINT('Ctrl Pts',(-82.6765109016597,29.0682605020227,205.542793856741));
#33317=CARTESIAN_POINT('Ctrl Pts',(-82.7657359477164,29.0682605020227,205.488310702079));
#33318=CARTESIAN_POINT('Ctrl Pts',(-82.8392357134513,29.0682605020227,205.439262575613));
#33319=CARTESIAN_POINT('Ctrl Pts',(-82.9183543749108,29.0682605020227,205.381517084423));
#33320=CARTESIAN_POINT('Ctrl Pts',(-83.0034121639627,29.0682605020227,205.315567580555));
#33321=CARTESIAN_POINT('Ctrl Pts',(-83.0932951769942,29.0682605020227,205.240278319977));
#33322=CARTESIAN_POINT('Ctrl Pts',(-83.1898372690957,29.0682605020227,205.157605307559));
#33323=CARTESIAN_POINT('Ctrl Pts',(-83.2912533102384,29.0682605020227,205.065413484233));
#33324=CARTESIAN_POINT('Ctrl Pts',(-83.3605669592593,29.0682605020227,205.000764852468));
#33325=CARTESIAN_POINT('Ctrl Pts',(-83.396483555646,29.0682605020227,204.96726555115));
#33326=CARTESIAN_POINT('',(-82.1407744210305,28.8682605020227,205.67539856397));
#33327=CARTESIAN_POINT('Ctrl Pts',(-81.1003096774409,28.8682605020226,204.618106897304));
#33328=CARTESIAN_POINT('Ctrl Pts',(-81.1003096774409,29.1082605020227,204.618106897304));
#33329=CARTESIAN_POINT('Ctrl Pts',(-81.1012008428613,28.8682605020226,204.656487672198));
#33330=CARTESIAN_POINT('Ctrl Pts',(-81.1012008428613,29.1082605020227,204.656487672198));
#33331=CARTESIAN_POINT('Ctrl Pts',(-81.1029519510787,28.8682605020226,204.731904523843));
#33332=CARTESIAN_POINT('Ctrl Pts',(-81.1029519510787,29.1082605020227,204.731904523843));
#33333=CARTESIAN_POINT('Ctrl Pts',(-81.1182161233739,28.8682605020226,204.841928331133));
#33334=CARTESIAN_POINT('Ctrl Pts',(-81.1182161233739,29.1082605020227,204.841928331133));
#33335=CARTESIAN_POINT('Ctrl Pts',(-81.1416071069158,28.8682605020227,204.946917430261));
#33336=CARTESIAN_POINT('Ctrl Pts',(-81.1416071069158,29.1082605020227,204.946917430261));
#33337=CARTESIAN_POINT('Ctrl Pts',(-81.1762688598019,28.8682605020226,205.045681980795));
#33338=CARTESIAN_POINT('Ctrl Pts',(-81.1762688598019,29.1082605020227,205.045681980795));
#33339=CARTESIAN_POINT('Ctrl Pts',(-81.219761777561,28.8682605020227,205.139235584572));
#33340=CARTESIAN_POINT('Ctrl Pts',(-81.219761777561,29.1082605020227,205.139235584572));
#33341=CARTESIAN_POINT('Ctrl Pts',(-81.2738509190422,28.8682605020226,205.226419892733));
#33342=CARTESIAN_POINT('Ctrl Pts',(-81.2738509190422,29.1082605020227,205.226419892733));
#33343=CARTESIAN_POINT('Ctrl Pts',(-81.3359769680758,28.8682605020227,205.309343112776));
#33344=CARTESIAN_POINT('Ctrl Pts',(-81.3359769680758,29.1082605020227,205.309343112776));
#33345=CARTESIAN_POINT('Ctrl Pts',(-81.409257689452,28.8682605020227,205.383935517473));
#33346=CARTESIAN_POINT('Ctrl Pts',(-81.409257689452,29.1082605020227,205.383935517473));
#33347=CARTESIAN_POINT('Ctrl Pts',(-81.4874484042645,28.8682605020227,205.452457639886));
#33348=CARTESIAN_POINT('Ctrl Pts',(-81.4874484042645,29.1082605020227,205.452457639886));
#33349=CARTESIAN_POINT('Ctrl Pts',(-81.5709554302159,28.8682605020226,205.51151956653));
#33350=CARTESIAN_POINT('Ctrl Pts',(-81.5709554302159,29.1082605020227,205.51151956653));
#33351=CARTESIAN_POINT('Ctrl Pts',(-81.6573042663379,28.8682605020226,205.562384162401));
#33352=CARTESIAN_POINT('Ctrl Pts',(-81.6573042663379,29.1082605020227,205.562384162401));
#33353=CARTESIAN_POINT('Ctrl Pts',(-81.7471694226447,28.8682605020227,205.604015245344));
#33354=CARTESIAN_POINT('Ctrl Pts',(-81.7471694226447,29.1082605020227,205.604015245344));
#33355=CARTESIAN_POINT('Ctrl Pts',(-81.8408435437684,28.8682605020227,205.635573457601));
#33356=CARTESIAN_POINT('Ctrl Pts',(-81.8408435437684,29.1082605020227,205.635573457601));
#33357=CARTESIAN_POINT('Ctrl Pts',(-81.937428543862,28.8682605020227,205.658955068432));
#33358=CARTESIAN_POINT('Ctrl Pts',(-81.937428543862,29.1082605020227,205.658955068432));
#33359=CARTESIAN_POINT('Ctrl Pts',(-82.0380390792887,28.8682605020227,205.672321260714));
#33360=CARTESIAN_POINT('Ctrl Pts',(-82.0380390792887,29.1082605020227,205.672321260714));
#33361=CARTESIAN_POINT('Ctrl Pts',(-82.1061475940205,28.8682605020227,205.6743613625));
#33362=CARTESIAN_POINT('Ctrl Pts',(-82.1061475940205,29.1082605020227,205.6743613625));
#33363=CARTESIAN_POINT('Ctrl Pts',(-82.1407744210305,28.8682605020227,205.67539856397));
#33364=CARTESIAN_POINT('Ctrl Pts',(-82.1407744210305,29.1082605020227,205.67539856397));
#33365=CARTESIAN_POINT('',(-81.1003096774409,29.0682605020227,204.618106897304));
#33366=CARTESIAN_POINT('Ctrl Pts',(-81.1003096774409,29.0682605020227,204.618106897304));
#33367=CARTESIAN_POINT('Ctrl Pts',(-81.1012008428613,29.0682605020227,204.656487672198));
#33368=CARTESIAN_POINT('Ctrl Pts',(-81.1029519510787,29.0682605020227,204.731904523843));
#33369=CARTESIAN_POINT('Ctrl Pts',(-81.1182161233739,29.0682605020226,204.841928331133));
#33370=CARTESIAN_POINT('Ctrl Pts',(-81.1416071069158,29.0682605020227,204.946917430261));
#33371=CARTESIAN_POINT('Ctrl Pts',(-81.1762688598019,29.0682605020227,205.045681980795));
#33372=CARTESIAN_POINT('Ctrl Pts',(-81.219761777561,29.0682605020227,205.139235584572));
#33373=CARTESIAN_POINT('Ctrl Pts',(-81.2738509190422,29.0682605020226,205.226419892733));
#33374=CARTESIAN_POINT('Ctrl Pts',(-81.3359769680758,29.0682605020227,205.309343112776));
#33375=CARTESIAN_POINT('Ctrl Pts',(-81.409257689452,29.0682605020227,205.383935517473));
#33376=CARTESIAN_POINT('Ctrl Pts',(-81.4874484042645,29.0682605020227,205.452457639886));
#33377=CARTESIAN_POINT('Ctrl Pts',(-81.5709554302159,29.0682605020227,205.51151956653));
#33378=CARTESIAN_POINT('Ctrl Pts',(-81.6573042663379,29.0682605020226,205.562384162401));
#33379=CARTESIAN_POINT('Ctrl Pts',(-81.7471694226447,29.0682605020227,205.604015245344));
#33380=CARTESIAN_POINT('Ctrl Pts',(-81.8408435437684,29.0682605020227,205.635573457601));
#33381=CARTESIAN_POINT('Ctrl Pts',(-81.937428543862,29.0682605020227,205.658955068432));
#33382=CARTESIAN_POINT('Ctrl Pts',(-82.0380390792887,29.0682605020227,205.672321260714));
#33383=CARTESIAN_POINT('Ctrl Pts',(-82.1061475940205,29.0682605020227,205.6743613625));
#33384=CARTESIAN_POINT('Ctrl Pts',(-82.1407744210305,29.0682605020227,205.67539856397));
#33385=CARTESIAN_POINT('',(-81.1003096774409,28.8682605020226,204.618106897304));
#33386=CARTESIAN_POINT('Ctrl Pts',(-82.2669763441076,28.8682605020227,203.476680615253));
#33387=CARTESIAN_POINT('Ctrl Pts',(-82.2669763441076,29.1082605020227,203.476680615253));
#33388=CARTESIAN_POINT('Ctrl Pts',(-82.2253054563398,28.8682605020227,203.47872776826));
#33389=CARTESIAN_POINT('Ctrl Pts',(-82.2253054563398,29.1082605020227,203.47872776826));
#33390=CARTESIAN_POINT('Ctrl Pts',(-82.1434649417649,28.8682605020227,203.482748322286));
#33391=CARTESIAN_POINT('Ctrl Pts',(-82.1434649417649,29.1082605020227,203.482748322286));
#33392=CARTESIAN_POINT('Ctrl Pts',(-82.0241410353658,28.8682605020227,203.501576611548));
#33393=CARTESIAN_POINT('Ctrl Pts',(-82.0241410353658,29.1082605020227,203.501576611548));
#33394=CARTESIAN_POINT('Ctrl Pts',(-81.9100862366409,28.8682605020227,203.528517488753));
#33395=CARTESIAN_POINT('Ctrl Pts',(-81.9100862366409,29.1082605020227,203.528517488753));
#33396=CARTESIAN_POINT('Ctrl Pts',(-81.8022163226713,28.8682605020227,203.566608942768));
#33397=CARTESIAN_POINT('Ctrl Pts',(-81.8022163226713,29.1082605020227,203.566608942768));
#33398=CARTESIAN_POINT('Ctrl Pts',(-81.6995775154409,28.8682605020226,203.613915220538));
#33399=CARTESIAN_POINT('Ctrl Pts',(-81.6995775154409,29.1082605020226,203.613915220538));
#33400=CARTESIAN_POINT('Ctrl Pts',(-81.6025774997497,28.8682605020227,203.670645247919));
#33401=CARTESIAN_POINT('Ctrl Pts',(-81.6025774997497,29.1082605020227,203.670645247919));
#33402=CARTESIAN_POINT('Ctrl Pts',(-81.511586311035,28.8682605020227,203.737839098432));
#33403=CARTESIAN_POINT('Ctrl Pts',(-81.511586311035,29.1082605020227,203.737839098432));
#33404=CARTESIAN_POINT('Ctrl Pts',(-81.4274474677396,28.8682605020226,203.814045832477));
#33405=CARTESIAN_POINT('Ctrl Pts',(-81.4274474677396,29.1082605020226,203.814045832477));
#33406=CARTESIAN_POINT('Ctrl Pts',(-81.3502598969403,28.8682605020227,203.896814471532));
#33407=CARTESIAN_POINT('Ctrl Pts',(-81.3502598969403,29.1082605020227,203.896814471532));
#33408=CARTESIAN_POINT('Ctrl Pts',(-81.2836046541341,28.8682605020227,203.986120411003));
#33409=CARTESIAN_POINT('Ctrl Pts',(-81.2836046541341,29.1082605020227,203.986120411003));
#33410=CARTESIAN_POINT('Ctrl Pts',(-81.2272869827721,28.8682605020226,204.07996543829));
#33411=CARTESIAN_POINT('Ctrl Pts',(-81.2272869827721,29.1082605020226,204.07996543829));
#33412=CARTESIAN_POINT('Ctrl Pts',(-81.1802057409483,28.8682605020227,204.178064837255));
#33413=CARTESIAN_POINT('Ctrl Pts',(-81.1802057409483,29.1082605020227,204.178064837255));
#33414=CARTESIAN_POINT('Ctrl Pts',(-81.1448658950257,28.8682605020226,204.281525400815));
#33415=CARTESIAN_POINT('Ctrl Pts',(-81.1448658950257,29.1082605020226,204.281525400815));
#33416=CARTESIAN_POINT('Ctrl Pts',(-81.1186442554211,28.8682605020226,204.389408258654));
#33417=CARTESIAN_POINT('Ctrl Pts',(-81.1186442554211,29.1082605020226,204.389408258654));
#33418=CARTESIAN_POINT('Ctrl Pts',(-81.1028679096996,28.8682605020227,204.502187395063));
#33419=CARTESIAN_POINT('Ctrl Pts',(-81.1028679096996,29.1082605020227,204.502187395063));
#33420=CARTESIAN_POINT('Ctrl Pts',(-81.1011721240953,28.8682605020226,204.57902741711));
#33421=CARTESIAN_POINT('Ctrl Pts',(-81.1011721240953,29.1082605020226,204.57902741711));
#33422=CARTESIAN_POINT('Ctrl Pts',(-81.1003096774409,28.8682605020226,204.618106897304));
#33423=CARTESIAN_POINT('Ctrl Pts',(-81.1003096774409,29.1082605020226,204.618106897304));
#33424=CARTESIAN_POINT('',(-82.2669763441076,29.0682605020227,203.476680615253));
#33425=CARTESIAN_POINT('Ctrl Pts',(-82.2669763441076,29.0682605020227,203.476680615253));
#33426=CARTESIAN_POINT('Ctrl Pts',(-82.2253054563398,29.0682605020227,203.47872776826));
#33427=CARTESIAN_POINT('Ctrl Pts',(-82.1434649417649,29.0682605020227,203.482748322286));
#33428=CARTESIAN_POINT('Ctrl Pts',(-82.0241410353658,29.0682605020227,203.501576611548));
#33429=CARTESIAN_POINT('Ctrl Pts',(-81.9100862366409,29.0682605020227,203.528517488753));
#33430=CARTESIAN_POINT('Ctrl Pts',(-81.8022163226713,29.0682605020227,203.566608942768));
#33431=CARTESIAN_POINT('Ctrl Pts',(-81.6995775154409,29.0682605020227,203.613915220538));
#33432=CARTESIAN_POINT('Ctrl Pts',(-81.6025774997497,29.0682605020227,203.670645247919));
#33433=CARTESIAN_POINT('Ctrl Pts',(-81.511586311035,29.0682605020227,203.737839098432));
#33434=CARTESIAN_POINT('Ctrl Pts',(-81.4274474677396,29.0682605020226,203.814045832477));
#33435=CARTESIAN_POINT('Ctrl Pts',(-81.3502598969403,29.0682605020227,203.896814471532));
#33436=CARTESIAN_POINT('Ctrl Pts',(-81.2836046541341,29.0682605020227,203.986120411003));
#33437=CARTESIAN_POINT('Ctrl Pts',(-81.2272869827721,29.0682605020226,204.07996543829));
#33438=CARTESIAN_POINT('Ctrl Pts',(-81.1802057409483,29.0682605020227,204.178064837255));
#33439=CARTESIAN_POINT('Ctrl Pts',(-81.1448658950257,29.0682605020226,204.281525400815));
#33440=CARTESIAN_POINT('Ctrl Pts',(-81.1186442554211,29.0682605020227,204.389408258654));
#33441=CARTESIAN_POINT('Ctrl Pts',(-81.1028679096996,29.0682605020227,204.502187395063));
#33442=CARTESIAN_POINT('Ctrl Pts',(-81.1011721240953,29.0682605020227,204.57902741711));
#33443=CARTESIAN_POINT('Ctrl Pts',(-81.1003096774409,29.0682605020227,204.618106897304));
#33444=CARTESIAN_POINT('',(-82.2669763441076,28.8682605020227,203.476680615253));
#33445=CARTESIAN_POINT('Origin',(-82.2669763441075,28.8682605020227,203.790783179355));
#33446=CARTESIAN_POINT('',(-82.2669763441075,29.0682605020227,203.790783179355));
#33447=CARTESIAN_POINT('',(-82.2669763441075,29.0682605020227,203.790783179355));
#33448=CARTESIAN_POINT('',(-82.2669763441075,28.8682605020227,203.790783179355));
#33449=CARTESIAN_POINT('Ctrl Pts',(-81.4592840364153,28.8682605020227,204.601981096022));
#33450=CARTESIAN_POINT('Ctrl Pts',(-81.4592840364153,29.1082605020227,204.601981096022));
#33451=CARTESIAN_POINT('Ctrl Pts',(-81.4599708546575,28.8682605020227,204.574603393385));
#33452=CARTESIAN_POINT('Ctrl Pts',(-81.4599708546575,29.1082605020227,204.574603393385));
#33453=CARTESIAN_POINT('Ctrl Pts',(-81.4613196522816,28.8682605020227,204.520838105856));
#33454=CARTESIAN_POINT('Ctrl Pts',(-81.4613196522816,29.1082605020227,204.520838105856));
#33455=CARTESIAN_POINT('Ctrl Pts',(-81.471536117869,28.8682605020226,204.442066315421));
#33456=CARTESIAN_POINT('Ctrl Pts',(-81.471536117869,29.1082605020226,204.442066315421));
#33457=CARTESIAN_POINT('Ctrl Pts',(-81.4870242844412,28.8682605020226,204.366402575227));
#33458=CARTESIAN_POINT('Ctrl Pts',(-81.4870242844412,29.1082605020226,204.366402575227));
#33459=CARTESIAN_POINT('Ctrl Pts',(-81.5116228732431,28.8682605020227,204.294975855603));
#33460=CARTESIAN_POINT('Ctrl Pts',(-81.5116228732431,29.1082605020227,204.294975855603));
#33461=CARTESIAN_POINT('Ctrl Pts',(-81.5406873285984,28.8682605020226,204.226239456265));
#33462=CARTESIAN_POINT('Ctrl Pts',(-81.5406873285984,29.1082605020226,204.226239456265));
#33463=CARTESIAN_POINT('Ctrl Pts',(-81.5776105868505,28.8682605020226,204.161660790704));
#33464=CARTESIAN_POINT('Ctrl Pts',(-81.5776105868505,29.1082605020226,204.161660790704));
#33465=CARTESIAN_POINT('Ctrl Pts',(-81.6205162333266,28.8682605020227,204.100167655303));
#33466=CARTESIAN_POINT('Ctrl Pts',(-81.6205162333266,29.1082605020227,204.100167655303));
#33467=CARTESIAN_POINT('Ctrl Pts',(-81.6702670801791,28.8682605020227,204.042771493033));
#33468=CARTESIAN_POINT('Ctrl Pts',(-81.6702670801791,29.1082605020227,204.042771493033));
#33469=CARTESIAN_POINT('Ctrl Pts',(-81.7261657529711,28.8682605020226,203.990350529552));
#33470=CARTESIAN_POINT('Ctrl Pts',(-81.7261657529711,29.1082605020226,203.990350529552));
#33471=CARTESIAN_POINT('Ctrl Pts',(-81.7877699492256,28.8682605020227,203.943644208757));
#33472=CARTESIAN_POINT('Ctrl Pts',(-81.7877699492256,29.1082605020227,203.943644208757));
#33473=CARTESIAN_POINT('Ctrl Pts',(-81.8546361678019,28.8682605020226,203.903103127741));
#33474=CARTESIAN_POINT('Ctrl Pts',(-81.8546361678019,29.1082605020226,203.903103127741));
#33475=CARTESIAN_POINT('Ctrl Pts',(-81.9264899768362,28.8682605020227,203.867682009478));
#33476=CARTESIAN_POINT('Ctrl Pts',(-81.9264899768362,29.1082605020227,203.867682009478));
#33477=CARTESIAN_POINT('Ctrl Pts',(-82.004046772439,28.8682605020227,203.838929655973));
#33478=CARTESIAN_POINT('Ctrl Pts',(-82.004046772439,29.1082605020227,203.838929655973));
#33479=CARTESIAN_POINT('Ctrl Pts',(-82.087013622034,28.8682605020227,203.816955559262));
#33480=CARTESIAN_POINT('Ctrl Pts',(-82.087013622034,29.1082605020227,203.816955559262));
#33481=CARTESIAN_POINT('Ctrl Pts',(-82.1750352431015,28.8682605020227,203.799568977673));
#33482=CARTESIAN_POINT('Ctrl Pts',(-82.1750352431015,29.1082605020227,203.799568977673));
#33483=CARTESIAN_POINT('Ctrl Pts',(-82.2358202943267,28.8682605020227,203.793760419858));
#33484=CARTESIAN_POINT('Ctrl Pts',(-82.2358202943267,29.1082605020227,203.793760419858));
#33485=CARTESIAN_POINT('Ctrl Pts',(-82.2669763441075,28.8682605020227,203.790783179355));
#33486=CARTESIAN_POINT('Ctrl Pts',(-82.2669763441075,29.1082605020227,203.790783179355));
#33487=CARTESIAN_POINT('Ctrl Pts',(-81.4592840364153,29.0682605020227,204.601981096022));
#33488=CARTESIAN_POINT('Ctrl Pts',(-81.4599708546575,29.0682605020227,204.574603393385));
#33489=CARTESIAN_POINT('Ctrl Pts',(-81.4613196522816,29.0682605020227,204.520838105856));
#33490=CARTESIAN_POINT('Ctrl Pts',(-81.471536117869,29.0682605020227,204.442066315421));
#33491=CARTESIAN_POINT('Ctrl Pts',(-81.4870242844412,29.0682605020227,204.366402575227));
#33492=CARTESIAN_POINT('Ctrl Pts',(-81.5116228732431,29.0682605020227,204.294975855603));
#33493=CARTESIAN_POINT('Ctrl Pts',(-81.5406873285984,29.0682605020227,204.226239456265));
#33494=CARTESIAN_POINT('Ctrl Pts',(-81.5776105868505,29.0682605020227,204.161660790704));
#33495=CARTESIAN_POINT('Ctrl Pts',(-81.6205162333266,29.0682605020227,204.100167655303));
#33496=CARTESIAN_POINT('Ctrl Pts',(-81.6702670801791,29.0682605020227,204.042771493033));
#33497=CARTESIAN_POINT('Ctrl Pts',(-81.7261657529711,29.0682605020227,203.990350529552));
#33498=CARTESIAN_POINT('Ctrl Pts',(-81.7877699492256,29.0682605020227,203.943644208757));
#33499=CARTESIAN_POINT('Ctrl Pts',(-81.8546361678019,29.0682605020227,203.903103127741));
#33500=CARTESIAN_POINT('Ctrl Pts',(-81.9264899768362,29.0682605020227,203.867682009478));
#33501=CARTESIAN_POINT('Ctrl Pts',(-82.004046772439,29.0682605020227,203.838929655973));
#33502=CARTESIAN_POINT('Ctrl Pts',(-82.087013622034,29.0682605020227,203.816955559262));
#33503=CARTESIAN_POINT('Ctrl Pts',(-82.1750352431015,29.0682605020227,203.799568977673));
#33504=CARTESIAN_POINT('Ctrl Pts',(-82.2358202943267,29.0682605020227,203.793760419858));
#33505=CARTESIAN_POINT('Ctrl Pts',(-82.2669763441075,29.0682605020227,203.790783179355));
#33506=CARTESIAN_POINT('Origin',(18.6572199957115,29.0682605020217,207.25));
#33507=CARTESIAN_POINT('',(5.90651941603066,31.2638292831994,207.25));
#33508=CARTESIAN_POINT('',(-84.3160797324307,31.2638292832004,207.250000000001));
#33509=CARTESIAN_POINT('',(18.6572199957116,31.2638292831994,207.25));
#33510=CARTESIAN_POINT('',(8.28134461617001,29.0682605020218,207.25));
#33511=CARTESIAN_POINT('',(6.39609118240601,30.8112113446932,207.25));
#33512=CARTESIAN_POINT('',(-86.2573680265828,29.0682605020227,207.250000000001));
#33513=CARTESIAN_POINT('',(18.6572199957115,29.0682605020217,207.25));
#33514=CARTESIAN_POINT('',(-86.2573680265828,29.6774440008114,207.250000000001));
#33515=CARTESIAN_POINT('',(-86.2573680265828,29.0682605020227,207.250000000001));
#33516=CARTESIAN_POINT('',(-52.899264332329,56.9370761267468,207.25));
#33517=CARTESIAN_POINT('Origin',(18.6572199957116,31.2638292831994,207.25));
#33518=CARTESIAN_POINT('',(5.90651941603069,31.2638292831994,210.5));
#33519=CARTESIAN_POINT('',(-84.3160797324307,31.2638292832004,210.500000000001));
#33520=CARTESIAN_POINT('',(18.6572199957116,31.2638292831994,210.5));
#33521=CARTESIAN_POINT('',(5.9065194160306,31.2638292831994,197.5));
#33522=CARTESIAN_POINT('',(-84.3160797324308,31.2638292832004,197.500000000001));
#33523=CARTESIAN_POINT('Origin',(18.6572199957116,31.2638292831994,210.5));
#33524=CARTESIAN_POINT('',(4.59583969805239,32.4755763502034,210.5));
#33525=CARTESIAN_POINT('',(-82.8332429822645,32.4755763502043,210.5));
#33526=CARTESIAN_POINT('',(18.6572199957116,32.4755763502033,210.5));
#33527=CARTESIAN_POINT('',(6.39609118240604,30.8112113446932,210.5));
#33528=CARTESIAN_POINT('',(-52.899264332329,56.9370761267468,210.5));
#33529=CARTESIAN_POINT('Origin',(18.6572199957115,31.2755763502033,198.2));
#33530=CARTESIAN_POINT('',(5.8938132639902,31.2755763502035,198.2));
#33531=CARTESIAN_POINT('',(-84.3017046345787,31.2755763502044,198.200000000001));
#33532=CARTESIAN_POINT('',(18.6572199957115,31.2755763502033,198.2));
#33533=CARTESIAN_POINT('',(4.5958396980523,32.4755763502034,198.2));
#33534=CARTESIAN_POINT('',(6.39609118240595,30.8112113446932,198.2));
#33535=CARTESIAN_POINT('',(-82.8332429822646,32.4755763502043,198.200000000001));
#33536=CARTESIAN_POINT('',(18.6572199957115,32.4755763502033,198.2));
#33537=CARTESIAN_POINT('',(-52.8992643323291,56.9370761267468,198.2));
#33538=CARTESIAN_POINT('Origin',(18.6572199957115,31.2755763502033,199.2));
#33539=CARTESIAN_POINT('',(5.89381326399021,31.2755763502035,199.2));
#33540=CARTESIAN_POINT('',(-84.3017046345787,31.2755763502044,199.200000000001));
#33541=CARTESIAN_POINT('',(18.6572199957115,31.2755763502033,199.2));
#33542=CARTESIAN_POINT('',(5.8938132639902,31.2755763502035,197.5));
#33543=CARTESIAN_POINT('',(-84.3017046345787,31.2755763502044,197.500000000001));
#33544=CARTESIAN_POINT('Origin',(18.6572199957115,29.0682605020217,199.2));
#33545=CARTESIAN_POINT('',(-86.2573680265829,29.6774440008114,199.200000000001));
#33546=CARTESIAN_POINT('',(-86.2573680265829,29.0682605020227,199.200000000001));
#33547=CARTESIAN_POINT('',(-86.2573680265829,29.0682605020227,199.200000000001));
#33548=CARTESIAN_POINT('',(8.28134461616996,29.0682605020218,199.2));
#33549=CARTESIAN_POINT('',(18.6572199957115,29.0682605020217,199.2));
#33550=CARTESIAN_POINT('',(6.39609118240596,30.8112113446932,199.2));
#33551=CARTESIAN_POINT('',(-52.8992643323291,56.9370761267468,199.2));
#33552=CARTESIAN_POINT('Origin',(18.6572199957116,30.6104283104369,212.5));
#33553=CARTESIAN_POINT('',(6.61326707486714,30.6104283104371,211.828238018329));
#33554=CARTESIAN_POINT('',(-85.1156582925022,30.610428310438,211.82823801833));
#33555=CARTESIAN_POINT('',(18.6572199957116,30.6104283104369,211.828238018329));
#33556=CARTESIAN_POINT('',(6.61326707486715,30.6104283104371,212.5));
#33557=CARTESIAN_POINT('',(6.61326707486704,30.6104283104371,197.5));
#33558=CARTESIAN_POINT('',(-85.1156582925022,30.610428310438,212.500000000001));
#33559=CARTESIAN_POINT('',(-13.7460461167398,30.6104283104372,212.5));
#33560=CARTESIAN_POINT('',(-85.1156582925023,30.610428310438,197.500000000001));
#33561=CARTESIAN_POINT('Origin',(18.6572199957116,30.6104283104369,211.828238018329));
#33562=CARTESIAN_POINT('',(-86.2573680265828,29.6774440008114,211.82823801833));
#33563=CARTESIAN_POINT('',(-86.2573680265828,26.8977681671301,211.82823801833));
#33564=CARTESIAN_POINT('',(-86.2573680265828,30.610428310438,211.82823801833));
#33565=CARTESIAN_POINT('',(-78.2291940435082,19.4755763502051,211.82823801833));
#33566=CARTESIAN_POINT('',(-38.2529492465526,-17.4831838397085,211.82823801833));
#33567=CARTESIAN_POINT('',(18.6572199957114,19.4755763502041,211.828238018329));
#33568=CARTESIAN_POINT('',(18.6572199957114,19.4755763502041,211.828238018329));
#33569=CARTESIAN_POINT('',(6.39609118240605,30.8112113446932,211.828238018329));
#33570=CARTESIAN_POINT('',(-52.899264332329,56.9370761267468,211.82823801833));
#33571=CARTESIAN_POINT('Origin',(-38.2529492465528,-17.4831838397084,197.5));
#33572=CARTESIAN_POINT('',(-48.4539024103773,-8.05221843499776,205.));
#33573=CARTESIAN_POINT('Origin',(-47.2790611019306,-9.13838043947375,205.));
#33574=CARTESIAN_POINT('Origin',(-38.2529492465527,-17.4831838397085,197.5));
#33575=CARTESIAN_POINT('',(-80.7620383926607,21.8172366880922,205.));
#33576=CARTESIAN_POINT('Origin',(-79.587197084214,20.7310746836162,205.));
#33577=CARTESIAN_POINT('Origin',(-47.6184867283294,-9.50551834836335,205.));
#33578=CARTESIAN_POINT('',(-48.793328036776,-8.41935634388735,205.));
#33579=CARTESIAN_POINT('Origin',(-47.6184867283294,-9.50551834836335,205.));
#33580=CARTESIAN_POINT('',(-48.793328036776,-8.41935634388735,205.));
#33581=CARTESIAN_POINT('Origin',(-79.9266227106128,20.3639367747266,205.));
#33582=CARTESIAN_POINT('',(-81.1014640190594,21.4500987792026,205.));
#33583=CARTESIAN_POINT('Origin',(-79.9266227106128,20.3639367747266,205.));
#33584=CARTESIAN_POINT('',(-81.1014640190594,21.4500987792026,205.));
#33585=CARTESIAN_POINT('Origin',(-43.9471076394335,-12.8997746123508,209.));
#33586=CARTESIAN_POINT('',(-43.6076820130347,-12.5326367034613,209.));
#33587=CARTESIAN_POINT('',(-55.1735654967775,-1.83976857061746,209.));
#33588=CARTESIAN_POINT('',(-43.6076820130347,-12.5326367034613,209.));
#33589=CARTESIAN_POINT('',(-78.2291940435082,19.4755763502051,209.));
#33590=CARTESIAN_POINT('',(-43.6076820130347,-12.5326367034613,209.));
#33591=CARTESIAN_POINT('',(-83.2585761731098,24.1253309476037,209.));
#33592=CARTESIAN_POINT('',(-43.6076820130347,-12.5326367034613,209.));
#33593=CARTESIAN_POINT('',(-83.5980017995085,23.7581930387141,209.));
#33594=CARTESIAN_POINT('',(-83.5980017995085,23.7581930387141,209.));
#33595=CARTESIAN_POINT('',(-43.9471076394335,-12.8997746123508,209.));
#33596=CARTESIAN_POINT('',(-43.9471076394335,-12.8997746123508,209.));
#33597=CARTESIAN_POINT('',(-43.9471076394335,-12.8997746123508,209.));
#33598=CARTESIAN_POINT('Origin',(-43.9471076394335,-12.8997746123508,209.));
#33599=CARTESIAN_POINT('',(-43.6076820130348,-12.5326367034613,201.));
#33600=CARTESIAN_POINT('',(-43.6076820130347,-12.5326367034613,209.));
#33601=CARTESIAN_POINT('',(-43.9471076394335,-12.8997746123508,201.));
#33602=CARTESIAN_POINT('',(-43.9471076394335,-12.8997746123508,209.));
#33603=CARTESIAN_POINT('',(-43.9471076394335,-12.8997746123508,201.));
#33604=CARTESIAN_POINT('Origin',(-43.9471076394335,-12.8997746123508,201.));
#33605=CARTESIAN_POINT('',(-83.2585761731099,24.1253309476037,201.000000000001));
#33606=CARTESIAN_POINT('',(-78.2291940435083,19.4755763502051,201.));
#33607=CARTESIAN_POINT('',(-43.6076820130348,-12.5326367034613,201.));
#33608=CARTESIAN_POINT('',(-55.1735654967775,-1.8397685706175,201.));
#33609=CARTESIAN_POINT('',(-43.6076820130348,-12.5326367034613,201.));
#33610=CARTESIAN_POINT('',(-38.2529492465527,-17.4831838397084,201.));
#33611=CARTESIAN_POINT('',(-83.5980017995086,23.7581930387141,201.000000000001));
#33612=CARTESIAN_POINT('',(-43.9471076394335,-12.8997746123508,201.));
#33613=CARTESIAN_POINT('',(-83.5980017995086,23.7581930387141,201.000000000001));
#33614=CARTESIAN_POINT('Origin',(-83.5980017995085,23.7581930387141,209.));
#33615=CARTESIAN_POINT('',(-83.2585761731098,24.1253309476037,209.));
#33616=CARTESIAN_POINT('',(-83.5980017995085,23.7581930387141,209.));
#33617=CARTESIAN_POINT('Origin',(-38.5923748729513,-17.8503217485981,212.5));
#33618=CARTESIAN_POINT('Origin',(-38.2529492465526,-17.4831838397085,212.5));
#33619=CARTESIAN_POINT('',(-78.2291940435084,19.4755763502051,197.5));
#33620=CARTESIAN_POINT('',(-55.1735654967776,-1.8397685706175,197.5));
#33621=CARTESIAN_POINT('Origin',(-13.74604611674,9.02457653154,212.5));
#33622=CARTESIAN_POINT('',(-55.1735654967775,-1.8397685706175,212.5));
#33623=CARTESIAN_POINT('',(41.7128485424422,-1.8397685706175,212.5));
#33624=CARTESIAN_POINT('',(-13.74604611674,-1.8397685706175,212.5));
#33625=CARTESIAN_POINT('',(-41.1121851991166,-14.8397685706175,212.5));
#33626=CARTESIAN_POINT('',(-38.2529492465526,-17.4831838397084,212.5));
#33627=CARTESIAN_POINT('',(55.7742288401031,-14.8397685706175,212.499999999999));
#33628=CARTESIAN_POINT('',(-13.74604611674,-14.8397685706175,212.5));
#33629=CARTESIAN_POINT('',(6.39609118240605,30.8112113446932,212.5));
#33630=CARTESIAN_POINT('',(38.4592255574052,-7.8397685706175,212.5));
#33631=CARTESIAN_POINT('Origin',(40.4592255574052,-7.8397685706175,212.5));
#33632=CARTESIAN_POINT('',(-39.5407744425949,-7.8397685706175,212.5));
#33633=CARTESIAN_POINT('Origin',(-37.5407744425949,-7.8397685706175,212.5));
#33634=CARTESIAN_POINT('Origin',(-13.7460461167401,9.02457653154,197.5));
#33635=CARTESIAN_POINT('',(-55.1735654967776,-1.8397685706175,197.5));
#33636=CARTESIAN_POINT('',(41.7128485424421,-1.8397685706175,197.5));
#33637=CARTESIAN_POINT('',(-13.7460461167401,-1.8397685706175,197.5));
#33638=CARTESIAN_POINT('',(55.774228840103,-14.8397685706175,197.5));
#33639=CARTESIAN_POINT('',(6.39609118240595,30.8112113446932,197.5));
#33640=CARTESIAN_POINT('',(-41.1121851991167,-14.8397685706175,197.5));
#33641=CARTESIAN_POINT('',(-13.7460461167401,-14.8397685706175,197.5));
#33642=CARTESIAN_POINT('',(-38.2529492465528,-17.4831838397084,197.5));
#33643=CARTESIAN_POINT('',(38.4592255574051,-7.8397685706175,197.5));
#33644=CARTESIAN_POINT('Origin',(40.4592255574051,-7.8397685706175,197.5));
#33645=CARTESIAN_POINT('',(-39.540774442595,-7.8397685706175,197.5));
#33646=CARTESIAN_POINT('Origin',(-37.540774442595,-7.8397685706175,197.5));
#33647=CARTESIAN_POINT('Origin',(-38.2529492465528,-17.4831838397084,197.5));
#33648=CARTESIAN_POINT('',(-55.1735654967776,-1.8397685706175,197.5));
#33649=CARTESIAN_POINT('',(-41.1121851991167,-14.8397685706175,197.5));
#33650=CARTESIAN_POINT('',(-55.1735654967776,-1.8397685706175,197.5));
#33651=CARTESIAN_POINT('Origin',(-37.540774442595,-7.8397685706175,197.5));
#33652=CARTESIAN_POINT('',(-39.540774442595,-7.8397685706175,197.5));
#33653=CARTESIAN_POINT('Origin',(40.4592255574051,-7.8397685706175,197.5));
#33654=CARTESIAN_POINT('',(38.4592255574051,-7.8397685706175,197.5));
#33655=CARTESIAN_POINT('Origin',(-13.7460461167401,-14.8397685706175,197.5));
#33656=CARTESIAN_POINT('',(55.774228840103,-14.8397685706175,197.5));
#33657=CARTESIAN_POINT('Origin',(6.39609118240595,30.8112113446932,197.5));
#33658=CARTESIAN_POINT('',(50.7515564684729,-10.1962172656254,209.));
#33659=CARTESIAN_POINT('',(50.7515564684727,-10.1962172656254,199.));
#33660=CARTESIAN_POINT('',(50.7515564684728,-10.1962172656254,199.));
#33661=CARTESIAN_POINT('',(41.7128485424422,-1.8397685706175,209.));
#33662=CARTESIAN_POINT('',(50.7515564684729,-10.1962172656254,209.));
#33663=CARTESIAN_POINT('',(41.7128485424421,-1.8397685706175,197.5));
#33664=CARTESIAN_POINT('',(41.7128485424422,-1.83976857061742,199.));
#33665=CARTESIAN_POINT('',(41.7128485424421,-1.8397685706175,197.5));
#33666=CARTESIAN_POINT('',(50.7515564684728,-10.1962172656254,199.));
#33667=CARTESIAN_POINT('Origin',(-13.7460461167401,-1.8397685706175,197.5));
#33668=CARTESIAN_POINT('',(41.7128485424421,-1.8397685706175,197.5));
#33669=CARTESIAN_POINT('Origin',(6.39609118240595,30.8112113446932,197.5));
#33670=CARTESIAN_POINT('',(48.9892945058029,-8.56697425891133,205.));
#33671=CARTESIAN_POINT('Origin',(47.8144531973563,-7.48081225443535,205.));
#33672=CARTESIAN_POINT('Origin',(6.39609118240595,30.8112113446932,197.5));
#33673=CARTESIAN_POINT('',(15.2126068879612,22.6601833697736,205.));
#33674=CARTESIAN_POINT('Origin',(14.0377655795145,23.7463453742496,205.));
#33675=CARTESIAN_POINT('Origin',(48.0181085731954,-7.2605295091016,205.));
#33676=CARTESIAN_POINT('',(49.1929498816421,-8.3466915135776,205.));
#33677=CARTESIAN_POINT('Origin',(48.0181085731954,-7.2605295091016,205.));
#33678=CARTESIAN_POINT('',(49.1929498816421,-8.3466915135776,205.));
#33679=CARTESIAN_POINT('Origin',(14.2414209553537,23.9666281195834,205.));
#33680=CARTESIAN_POINT('',(15.4162622638004,22.8804661151074,205.));
#33681=CARTESIAN_POINT('Origin',(14.2414209553537,23.9666281195834,205.));
#33682=CARTESIAN_POINT('',(15.4162622638004,22.8804661151074,205.));
#33683=CARTESIAN_POINT('Origin',(50.9552118443121,-9.9759345202916,199.));
#33684=CARTESIAN_POINT('',(18.6572199957115,19.4755763502051,199.));
#33685=CARTESIAN_POINT('',(50.7515564684728,-10.1962172656254,199.));
#33686=CARTESIAN_POINT('',(9.63211067283946,27.8194528910347,199.));
#33687=CARTESIAN_POINT('',(50.7515564684728,-10.1962172656254,199.));
#33688=CARTESIAN_POINT('',(9.83576604867871,28.0397356363684,199.));
#33689=CARTESIAN_POINT('',(9.83576604867871,28.0397356363684,199.));
#33690=CARTESIAN_POINT('',(50.9552118443121,-9.9759345202916,199.));
#33691=CARTESIAN_POINT('',(50.9552118443121,-9.9759345202916,199.));
#33692=CARTESIAN_POINT('',(50.9552118443121,-9.9759345202916,199.));
#33693=CARTESIAN_POINT('Origin',(50.9552118443121,-9.9759345202916,199.));
#33694=CARTESIAN_POINT('',(50.9552118443122,-9.9759345202916,209.));
#33695=CARTESIAN_POINT('',(50.9552118443121,-9.9759345202916,199.));
#33696=CARTESIAN_POINT('',(50.9552118443122,-9.9759345202916,209.));
#33697=CARTESIAN_POINT('Origin',(50.9552118443122,-9.9759345202916,209.));
#33698=CARTESIAN_POINT('',(9.63211067283953,27.8194528910346,209.));
#33699=CARTESIAN_POINT('',(18.6572199957114,19.4755763502051,209.));
#33700=CARTESIAN_POINT('',(50.7515564684729,-10.1962172656254,209.));
#33701=CARTESIAN_POINT('',(50.7515564684729,-10.1962172656254,209.));
#33702=CARTESIAN_POINT('',(9.83576604867877,28.0397356363684,209.));
#33703=CARTESIAN_POINT('',(50.9552118443122,-9.9759345202916,209.));
#33704=CARTESIAN_POINT('',(9.83576604867877,28.0397356363684,209.));
#33705=CARTESIAN_POINT('Origin',(9.83576604867871,28.0397356363684,199.));
#33706=CARTESIAN_POINT('',(9.63211067283946,27.8194528910347,199.));
#33707=CARTESIAN_POINT('',(9.83576604867871,28.0397356363684,199.));
#33708=CARTESIAN_POINT('Origin',(6.5997465582453,31.031494090027,212.5));
#33709=CARTESIAN_POINT('Origin',(-13.74604611674,9.02457653154,212.5));
#33710=CARTESIAN_POINT('',(-82.8332429822645,32.4755763502051,212.5));
#33711=CARTESIAN_POINT('',(-52.899264332329,56.9370761267468,212.5));
#33712=CARTESIAN_POINT('',(4.59583969805065,32.4755763502051,212.5));
#33713=CARTESIAN_POINT('',(6.39609118240605,30.8112113446932,212.5));
#33714=CARTESIAN_POINT('',(-13.74604611674,32.4755763502051,212.5));
#33715=CARTESIAN_POINT('Origin',(-13.7460461167401,9.02457653154,197.5));
#33716=CARTESIAN_POINT('',(-86.2573680265831,26.8977681671302,197.500000000001));
#33717=CARTESIAN_POINT('',(-86.2573680265831,29.6774440008112,197.500000000001));
#33718=CARTESIAN_POINT('',(-86.2573680265831,9.02457653154,197.500000000001));
#33719=CARTESIAN_POINT('',(-82.8332429822646,32.4755763502051,197.500000000001));
#33720=CARTESIAN_POINT('',(-52.8992643323291,56.9370761267468,197.5));
#33721=CARTESIAN_POINT('',(4.59583969805055,32.4755763502051,197.5));
#33722=CARTESIAN_POINT('',(-13.7460461167401,32.4755763502051,197.5));
#33723=CARTESIAN_POINT('',(18.6572199957114,19.4755763502051,197.5));
#33724=CARTESIAN_POINT('',(6.39609118240595,30.8112113446932,197.5));
#33725=CARTESIAN_POINT('',(-78.2291940435083,19.4755763502051,197.5));
#33726=CARTESIAN_POINT('',(-13.7460461167401,19.4755763502051,197.5));
#33727=CARTESIAN_POINT('',(-38.2529492465527,-17.4831838397085,197.5));
#33728=CARTESIAN_POINT('Origin',(-38.2529492465527,-17.4831838397085,197.5));
#33729=CARTESIAN_POINT('',(-78.2291940435083,19.4755763502051,197.5));
#33730=CARTESIAN_POINT('',(-86.2573680265831,26.8977681671302,197.500000000001));
#33731=CARTESIAN_POINT('',(-78.2291940435083,19.4755763502051,197.5));
#33732=CARTESIAN_POINT('Origin',(-13.7460461167401,19.4755763502051,197.5));
#33733=CARTESIAN_POINT('',(18.6572199957114,19.4755763502051,197.5));
#33734=CARTESIAN_POINT('',(18.6572199957114,19.4755763502051,197.5));
#33735=CARTESIAN_POINT('',(18.6572199957114,19.4755763502051,197.5));
#33736=CARTESIAN_POINT('Origin',(6.39609118240595,30.8112113446932,197.5));
#33737=CARTESIAN_POINT('',(4.59583969805055,32.4755763502051,197.5));
#33738=CARTESIAN_POINT('',(8.28134461616995,29.0682605020218,197.5));
#33739=CARTESIAN_POINT('',(4.59583969805055,32.4755763502051,197.5));
#33740=CARTESIAN_POINT('Origin',(-13.7460461167401,32.4755763502051,197.5));
#33741=CARTESIAN_POINT('',(-82.8332429822646,32.4755763502051,197.500000000001));
#33742=CARTESIAN_POINT('Origin',(-52.8992643323291,56.9370761267468,197.5));
#33743=CARTESIAN_POINT('',(-86.2573680265831,29.6774440008112,197.500000000001));
#33744=CARTESIAN_POINT('Origin',(-86.2573680265831,9.02457653154,197.500000000001));
#33745=CARTESIAN_POINT('',(-86.2573680265829,29.0682605020227,199.200000000001));
#33746=CARTESIAN_POINT('',(-86.2573680265831,29.6774440008112,197.500000000001));
#33747=CARTESIAN_POINT('Origin',(6.39609118240605,30.8112113446933,212.5));
#33748=CARTESIAN_POINT('Origin',(-13.7460461167401,32.4755763502051,197.5));
#33749=CARTESIAN_POINT('',(-82.8332429822646,32.4755763502051,197.500000000001));
#33750=CARTESIAN_POINT('Origin',(-52.8992643323291,56.9370761267468,197.5));
#33751=CARTESIAN_POINT('Origin',(18.6572199957115,29.0682605020217,199.2));
#33752=CARTESIAN_POINT('',(0.,0.,0.));
#33753=CARTESIAN_POINT('Origin',(25.187903481163,63.761980950099,202.2));
#33754=CARTESIAN_POINT('',(21.2239277116833,64.2976077782208,202.2));
#33755=CARTESIAN_POINT('Origin',(25.18790348116,63.761980950101,202.2));
#33756=CARTESIAN_POINT('',(21.587903481163,63.761980950099,202.2));
#33757=CARTESIAN_POINT('Origin',(25.187903481163,63.761980950099,202.2));
#33758=CARTESIAN_POINT('Origin',(25.187903481163,63.761980950099,202.6));
#33759=CARTESIAN_POINT('',(21.2239277116865,64.2976077782203,202.6));
#33760=CARTESIAN_POINT('',(21.187903481163,63.761980950099,202.6));
#33761=CARTESIAN_POINT('Origin',(25.187903481163,63.761980950099,202.6));
#33762=CARTESIAN_POINT('Origin',(25.187903481163,63.761980950099,202.6));
#33763=CARTESIAN_POINT('',(21.187903481163,63.761980950099,202.6));
#33764=CARTESIAN_POINT('Origin',(25.18790348116,63.761980950101,211.3));
#33765=CARTESIAN_POINT('',(21.2239277116833,64.2976077782208,211.3));
#33766=CARTESIAN_POINT('Origin',(25.187903481163,63.761980950099,212.5));
#33767=CARTESIAN_POINT('',(26.787903481163,63.7619809500987,203.));
#33768=CARTESIAN_POINT('',(26.787903481163,63.761980950099,202.912499998088));
#33769=CARTESIAN_POINT('',(26.787903481163,63.761980950099,212.5));
#33770=CARTESIAN_POINT('',(26.787903481163,63.761980950099,202.6));
#33771=CARTESIAN_POINT('',(26.787903481163,63.761980950099,202.606249999044));
#33772=CARTESIAN_POINT('',(23.7486592957405,64.4609631921677,202.6));
#33773=CARTESIAN_POINT('Origin',(25.187903481163,63.761980950099,202.6));
#33774=CARTESIAN_POINT('Ctrl Pts',(26.787903481163,63.7619809500983,203.));
#33775=CARTESIAN_POINT('Ctrl Pts',(26.787903481163,63.7112520004935,202.996796584235));
#33776=CARTESIAN_POINT('Ctrl Pts',(26.7854910924781,63.6604721236311,202.99350200086));
#33777=CARTESIAN_POINT('Ctrl Pts',(26.7604511514014,63.3983856951183,202.97603893493));
#33778=CARTESIAN_POINT('Ctrl Pts',(26.6983614293065,63.1931353440354,202.960814162487));
#33779=CARTESIAN_POINT('Ctrl Pts',(26.5003141481196,62.8236961479851,202.930264458459));
#33780=CARTESIAN_POINT('Ctrl Pts',(26.3681111928548,62.662010067521,202.915234457258));
#33781=CARTESIAN_POINT('Ctrl Pts',(26.0503971457733,62.3987480817403,202.887026747492));
#33782=CARTESIAN_POINT('Ctrl Pts',(25.8682694857742,62.2993104687815,202.874610021169));
#33783=CARTESIAN_POINT('Ctrl Pts',(25.4696943299171,62.1727174517791,202.845547249388));
#33784=CARTESIAN_POINT('Ctrl Pts',(25.2563670240156,62.1493873298679,202.829992133333));
#33785=CARTESIAN_POINT('Ctrl Pts',(24.8410914178345,62.1866934369787,202.799711620382));
#33786=CARTESIAN_POINT('Ctrl Pts',(24.6427688077468,62.2438637796842,202.78525059673));
#33787=CARTESIAN_POINT('Ctrl Pts',(24.2712058497153,62.4335018359131,202.758157464374));
#33788=CARTESIAN_POINT('Ctrl Pts',(24.1029599888896,62.5669294408852,202.744242838934));
#33789=CARTESIAN_POINT('Ctrl Pts',(23.8302633753762,62.8897168830665,202.713917494956));
#33790=CARTESIAN_POINT('Ctrl Pts',(23.7276898417191,63.0750963218571,202.69847155234));
#33791=CARTESIAN_POINT('Ctrl Pts',(23.6024417596993,63.4670668651279,202.669153183349));
#33792=CARTESIAN_POINT('Ctrl Pts',(23.5779451866174,63.668940007034,202.656238383051));
#33793=CARTESIAN_POINT('Ctrl Pts',(23.6054510774695,64.0753209334884,202.629573549099));
#33794=CARTESIAN_POINT('Ctrl Pts',(23.6588128449442,64.2759642406826,202.614957907494));
#33795=CARTESIAN_POINT('Ctrl Pts',(23.7486592957404,64.4609631921677,202.6));
#33796=CARTESIAN_POINT('Origin',(25.187903481163,63.761980950099,212.5));
#33797=CARTESIAN_POINT('',(26.787903481163,63.7619809500989,203.7));
#33798=CARTESIAN_POINT('',(26.787903481163,63.761980950099,203.612499998088));
#33799=CARTESIAN_POINT('',(26.787903481163,63.761980950099,212.5));
#33800=CARTESIAN_POINT('Ctrl Pts',(26.787903481163,63.761980950099,202.912499998088));
#33801=CARTESIAN_POINT('Ctrl Pts',(26.787903481163,63.8816035254339,202.920053886877));
#33802=CARTESIAN_POINT('Ctrl Pts',(26.7744883750838,64.0008235214565,202.928071446123));
#33803=CARTESIAN_POINT('Ctrl Pts',(26.7204285286892,64.2381005673036,202.945025874336));
#33804=CARTESIAN_POINT('Ctrl Pts',(26.6790200147457,64.3551822716112,202.953928998405));
#33805=CARTESIAN_POINT('Ctrl Pts',(26.5308024775844,64.6575072281504,202.978423884113));
#33806=CARTESIAN_POINT('Ctrl Pts',(26.3998178470323,64.8281102460966,202.99397255119));
#33807=CARTESIAN_POINT('Ctrl Pts',(26.0848356880736,65.1026820164517,203.02279484759));
#33808=CARTESIAN_POINT('Ctrl Pts',(25.9060478414617,65.2063614843149,203.03513530515));
#33809=CARTESIAN_POINT('Ctrl Pts',(25.5166022913437,65.3415259652012,203.063532376512));
#33810=CARTESIAN_POINT('Ctrl Pts',(25.3093537590403,65.3707793765029,203.07864424866));
#33811=CARTESIAN_POINT('Ctrl Pts',(24.8903683797337,65.3483380052435,203.109195265901));
#33812=CARTESIAN_POINT('Ctrl Pts',(24.682721061272,65.2949157615971,203.124336216205));
#33813=CARTESIAN_POINT('Ctrl Pts',(24.3089997865868,65.1142494804449,203.151586725818));
#33814=CARTESIAN_POINT('Ctrl Pts',(24.1448884786953,64.9921268833827,203.164512384635));
#33815=CARTESIAN_POINT('Ctrl Pts',(23.8662397612558,64.687836578348,203.193886681));
#33816=CARTESIAN_POINT('Ctrl Pts',(23.7563717425979,64.5067740759857,203.209325963837));
#33817=CARTESIAN_POINT('Ctrl Pts',(23.6116618059432,64.1095748583762,203.239684058295));
#33818=CARTESIAN_POINT('Ctrl Pts',(23.5794678262025,63.8970057212076,203.253665946361));
#33819=CARTESIAN_POINT('Ctrl Pts',(23.599697430425,63.4801535614309,203.280726733181));
#33820=CARTESIAN_POINT('Ctrl Pts',(23.6486804568962,63.2797206238055,203.295169448835));
#33821=CARTESIAN_POINT('Ctrl Pts',(23.8226994528204,62.9009738311223,203.325430874816));
#33822=CARTESIAN_POINT('Ctrl Pts',(23.9489389782711,62.7275242008688,203.34098630025));
#33823=CARTESIAN_POINT('Ctrl Pts',(24.256932832041,62.4445394311034,203.370085076132));
#33824=CARTESIAN_POINT('Ctrl Pts',(24.4338702113582,62.3358715183235,203.382518405498));
#33825=CARTESIAN_POINT('Ctrl Pts',(24.8203227249822,62.1910946963225,203.410697234617));
#33826=CARTESIAN_POINT('Ctrl Pts',(25.0262711719672,62.1567869763195,203.425714308876));
#33827=CARTESIAN_POINT('Ctrl Pts',(25.4452179976236,62.1686010277284,203.456262514913));
#33828=CARTESIAN_POINT('Ctrl Pts',(25.6541792260724,62.2167638482125,203.471499271154));
#33829=CARTESIAN_POINT('Ctrl Pts',(26.0324903692996,62.3879978620503,203.499084458681));
#33830=CARTESIAN_POINT('Ctrl Pts',(26.1997047745697,62.5060199489405,203.511744223034));
#33831=CARTESIAN_POINT('Ctrl Pts',(26.4855979882815,62.8029319913109,203.540916721447));
#33832=CARTESIAN_POINT('Ctrl Pts',(26.5997607566442,62.980676287076,203.556303046633));
#33833=CARTESIAN_POINT('Ctrl Pts',(26.7501748873287,63.3623426521135,203.585888242806));
#33834=CARTESIAN_POINT('Ctrl Pts',(26.787903481163,63.5613581222044,203.599831130809));
#33835=CARTESIAN_POINT('Ctrl Pts',(26.787903481163,63.761980950099,203.612499998088));
#33836=CARTESIAN_POINT('Ctrl Pts',(26.787903481163,63.7619809500988,203.7));
#33837=CARTESIAN_POINT('Ctrl Pts',(26.787903481163,63.6848495192057,203.695129328645));
#33838=CARTESIAN_POINT('Ctrl Pts',(26.7823272250583,63.6076663989242,203.690052092221));
#33839=CARTESIAN_POINT('Ctrl Pts',(26.7402499780708,63.3192289003551,203.670303865423));
#33840=CARTESIAN_POINT('Ctrl Pts',(26.667176531147,63.11581633677,203.654794696706));
#33841=CARTESIAN_POINT('Ctrl Pts',(26.4496343128889,62.7567934686976,203.624192006769));
#33842=CARTESIAN_POINT('Ctrl Pts',(26.3099733765155,62.602947229556,203.609385167843));
#33843=CARTESIAN_POINT('Ctrl Pts',(25.9781444640218,62.3552648464668,203.581646669462));
#33844=CARTESIAN_POINT('Ctrl Pts',(25.7886683527539,62.2645066921842,203.568805771887));
#33845=CARTESIAN_POINT('Ctrl Pts',(25.382369354266,62.1598394149872,203.539179803247));
#33846=CARTESIAN_POINT('Ctrl Pts',(25.1692663810009,62.1481911110961,203.52364104478));
#33847=CARTESIAN_POINT('Ctrl Pts',(24.7587322026718,62.207248987663,203.493706260943));
#33848=CARTESIAN_POINT('Ctrl Pts',(24.5646851694379,62.2743564463977,203.479556998103));
#33849=CARTESIAN_POINT('Ctrl Pts',(24.2046978751832,62.4820298420444,203.453307924564));
#33850=CARTESIAN_POINT('Ctrl Pts',(24.0437650457417,62.6235440783622,203.438509606632));
#33851=CARTESIAN_POINT('Ctrl Pts',(23.7885670062959,62.9585764544945,203.40804899226));
#33852=CARTESIAN_POINT('Ctrl Pts',(23.6957639269873,63.1478699907815,203.392712097927));
#33853=CARTESIAN_POINT('Ctrl Pts',(23.5895951555988,63.5459326838728,203.36370462364));
#33854=CARTESIAN_POINT('Ctrl Pts',(23.5751062397505,63.7503103057142,203.351203540277));
#33855=CARTESIAN_POINT('Ctrl Pts',(23.6247059389547,64.1650452428808,203.323205666452));
#33856=CARTESIAN_POINT('Ctrl Pts',(23.6927866095703,64.3707804740557,203.307731854955));
#33857=CARTESIAN_POINT('Ctrl Pts',(23.9018731775003,64.7359913494376,203.277046685596));
#33858=CARTESIAN_POINT('Ctrl Pts',(24.0380772095468,64.8935726524055,203.262130019003));
#33859=CARTESIAN_POINT('Ctrl Pts',(24.3632744096962,65.1486279853084,203.234167717085));
#33860=CARTESIAN_POINT('Ctrl Pts',(24.5492366279778,65.2435061649562,203.221569458045));
#33861=CARTESIAN_POINT('Ctrl Pts',(24.9519305603642,65.3586094432589,203.192206358808));
#33862=CARTESIAN_POINT('Ctrl Pts',(25.1652176392351,65.3757892043211,203.176654175974));
#33863=CARTESIAN_POINT('Ctrl Pts',(25.5781415174269,65.3270040389637,203.146545143189));
#33864=CARTESIAN_POINT('Ctrl Pts',(25.7742792068995,65.2645760304671,203.132243436665));
#33865=CARTESIAN_POINT('Ctrl Pts',(26.1397504343722,65.0654395529092,203.105594492995));
#33866=CARTESIAN_POINT('Ctrl Pts',(26.3041087678418,64.9278245374005,203.091258673341));
#33867=CARTESIAN_POINT('Ctrl Pts',(26.567675494015,64.598662470267,203.060863647025));
#33868=CARTESIAN_POINT('Ctrl Pts',(26.665181531593,64.4111833670911,203.045469867924));
#33869=CARTESIAN_POINT('Ctrl Pts',(26.7664096376625,64.0643397927398,203.019876890872));
#33870=CARTESIAN_POINT('Ctrl Pts',(26.7879034811631,63.913436868219,203.009564090714));
#33871=CARTESIAN_POINT('Ctrl Pts',(26.787903481163,63.7619809500983,203.));
#33872=CARTESIAN_POINT('Origin',(25.187903481163,63.761980950099,212.5));
#33873=CARTESIAN_POINT('',(26.787903481163,63.761980950099,204.4));
#33874=CARTESIAN_POINT('',(26.787903481163,63.761980950099,204.312499998088));
#33875=CARTESIAN_POINT('',(26.787903481163,63.761980950099,212.5));
#33876=CARTESIAN_POINT('Ctrl Pts',(26.787903481163,63.761980950099,203.612499998088));
#33877=CARTESIAN_POINT('Ctrl Pts',(26.787903481163,63.7733300716832,203.613216668851));
#33878=CARTESIAN_POINT('Ctrl Pts',(26.7877827289335,63.7846837908196,203.613938032363));
#33879=CARTESIAN_POINT('Ctrl Pts',(26.7831991936214,63.9999555727865,203.627699055248));
#33880=CARTESIAN_POINT('Ctrl Pts',(26.7399082191147,64.2011116260035,203.64197991125));
#33881=CARTESIAN_POINT('Ctrl Pts',(26.5771050844058,64.5835518640169,203.672065658149));
#33882=CARTESIAN_POINT('Ctrl Pts',(26.4562637840854,64.760046779607,203.687616576013));
#33883=CARTESIAN_POINT('Ctrl Pts',(26.1562407270751,65.0524095270444,203.717016947517));
#33884=CARTESIAN_POINT('Ctrl Pts',(25.9813472815784,65.1667299651493,203.729644720974));
#33885=CARTESIAN_POINT('Ctrl Pts',(25.5982921414466,65.3221582302966,203.757575824942));
#33886=CARTESIAN_POINT('Ctrl Pts',(25.3939258076125,65.3620110358385,203.772477536784));
#33887=CARTESIAN_POINT('Ctrl Pts',(24.9732446111159,65.3619496379482,203.803152207362));
#33888=CARTESIAN_POINT('Ctrl Pts',(24.7609557974199,65.3188140611529,203.818631600028));
#33889=CARTESIAN_POINT('Ctrl Pts',(24.3764131853069,65.1558088196326,203.846671165494));
#33890=CARTESIAN_POINT('Ctrl Pts',(24.2062081008249,65.0416531052197,203.859149307122));
#33891=CARTESIAN_POINT('Ctrl Pts',(23.913547622975,64.7517280732952,203.888127315167));
#33892=CARTESIAN_POINT('Ctrl Pts',(23.7954277427113,64.5771996837515,203.903454833022));
#33893=CARTESIAN_POINT('Ctrl Pts',(23.6315585215372,64.1895285406312,203.933909767209));
#33894=CARTESIAN_POINT('Ctrl Pts',(23.5886182636867,63.9795728728208,203.948733511963));
#33895=CARTESIAN_POINT('Ctrl Pts',(23.587236335398,63.5640341496619,203.975024203449));
#33896=CARTESIAN_POINT('Ctrl Pts',(23.625303899541,63.3623430739075,203.989099762005));
#33897=CARTESIAN_POINT('Ctrl Pts',(23.7779729029101,62.9766614093573,204.01902072395));
#33898=CARTESIAN_POINT('Ctrl Pts',(23.893872407819,62.7975518937715,204.034556578128));
#33899=CARTESIAN_POINT('Ctrl Pts',(24.1865671125536,62.4967695520657,204.064221448014));
#33900=CARTESIAN_POINT('Ctrl Pts',(24.3596325075858,62.377284721672,204.077105239598));
#33901=CARTESIAN_POINT('Ctrl Pts',(24.7395813264973,62.2123431202278,204.104809840977));
#33902=CARTESIAN_POINT('Ctrl Pts',(24.9424115787873,62.1675939414645,204.119599546873));
#33903=CARTESIAN_POINT('Ctrl Pts',(25.3619149100335,62.1571561117494,204.150188331443));
#33904=CARTESIAN_POINT('Ctrl Pts',(25.5746728096165,62.1947594878389,204.165701928288));
#33905=CARTESIAN_POINT('Ctrl Pts',(25.9632553978713,62.3476624489653,204.194036075348));
#33906=CARTESIAN_POINT('Ctrl Pts',(26.1367309575285,62.4576799835756,204.206395745681));
#33907=CARTESIAN_POINT('Ctrl Pts',(26.4365577261353,62.7401058325329,204.235161468695));
#33908=CARTESIAN_POINT('Ctrl Pts',(26.558803278173,62.9111085532163,204.250416763838));
#33909=CARTESIAN_POINT('Ctrl Pts',(26.7325552445008,63.2939238566396,204.280925371403));
#33910=CARTESIAN_POINT('Ctrl Pts',(26.7809711604346,63.5027300416431,204.295876162346));
#33911=CARTESIAN_POINT('Ctrl Pts',(26.7876732452454,63.7306306492175,204.310511905124));
#33912=CARTESIAN_POINT('Ctrl Pts',(26.787903481163,63.7463097723831,204.311510399483));
#33913=CARTESIAN_POINT('Ctrl Pts',(26.787903481163,63.761980950099,204.312499998088));
#33914=CARTESIAN_POINT('Ctrl Pts',(26.787903481163,63.761980950099,204.4));
#33915=CARTESIAN_POINT('Ctrl Pts',(26.787903481163,63.6561553187078,204.393317356291));
#33916=CARTESIAN_POINT('Ctrl Pts',(26.7774081135394,63.5503731163489,204.386254811413));
#33917=CARTESIAN_POINT('Ctrl Pts',(26.7143998470148,63.2374536009571,204.364197491824));
#33918=CARTESIAN_POINT('Ctrl Pts',(26.6311516236278,63.0392550331286,204.348646619481));
#33919=CARTESIAN_POINT('Ctrl Pts',(26.3965428914708,62.6937415201734,204.318274797402));
#33920=CARTESIAN_POINT('Ctrl Pts',(26.249996570115,62.547920352436,204.303723693502));
#33921=CARTESIAN_POINT('Ctrl Pts',(25.9044069654626,62.3158467831105,204.276469163685));
#33922=CARTESIAN_POINT('Ctrl Pts',(25.7072891036901,62.2339218190914,204.262871868309));
#33923=CARTESIAN_POINT('Ctrl Pts',(25.2936850910905,62.1517017382011,204.232713242391));
#33924=CARTESIAN_POINT('Ctrl Pts',(25.081437358254,62.1517468396757,204.217236845205));
#33925=CARTESIAN_POINT('Ctrl Pts',(24.6763013596086,62.2324626340137,204.187695678637));
#33926=CARTESIAN_POINT('Ctrl Pts',(24.4867652763709,62.3095640693849,204.174487767628));
#33927=CARTESIAN_POINT('Ctrl Pts',(24.1386002292873,62.5355834334685,204.147521650523));
#33928=CARTESIAN_POINT('Ctrl Pts',(23.9853316554284,62.6854757681625,204.132468379729));
#33929=CARTESIAN_POINT('Ctrl Pts',(23.7487956744408,63.0325102641257,204.101930246813));
#33930=CARTESIAN_POINT('Ctrl Pts',(23.6663233411312,63.2253504812696,204.086746029573));
#33931=CARTESIAN_POINT('Ctrl Pts',(23.5804723637616,63.6283119424464,204.058169962327));
#33932=CARTESIAN_POINT('Ctrl Pts',(23.5765460629297,63.8342757255467,204.045848824783));
#33933=CARTESIAN_POINT('Ctrl Pts',(23.6479380218796,64.2457884260673,204.017259918275));
#33934=CARTESIAN_POINT('Ctrl Pts',(23.7261388223897,64.446656433769,204.001724497607));
#33935=CARTESIAN_POINT('Ctrl Pts',(23.9523099047955,64.7990266290427,203.971227314556));
#33936=CARTESIAN_POINT('Ctrl Pts',(24.0954681173645,64.9489001045456,203.956543841598));
#33937=CARTESIAN_POINT('Ctrl Pts',(24.4341862593746,65.188821316822,203.929044273366));
#33938=CARTESIAN_POINT('Ctrl Pts',(24.6274289558628,65.2752091081056,203.915867934136));
#33939=CARTESIAN_POINT('Ctrl Pts',(25.0374183239758,65.3687748161157,203.885972876045));
#33940=CARTESIAN_POINT('Ctrl Pts',(25.2501752060529,65.3746029806471,203.870459353393));
#33941=CARTESIAN_POINT('Ctrl Pts',(25.6581670236846,65.3047454842163,203.840709950024));
#33942=CARTESIAN_POINT('Ctrl Pts',(25.8499410107935,65.23265975469,203.827066511306));
#33943=CARTESIAN_POINT('Ctrl Pts',(26.2041413290638,65.0159083960482,203.800465611367));
#33944=CARTESIAN_POINT('Ctrl Pts',(26.3613218928151,64.8701835151,203.785532881));
#33945=CARTESIAN_POINT('Ctrl Pts',(26.6073305316025,64.5291897122417,203.755030846558));
#33946=CARTESIAN_POINT('Ctrl Pts',(26.6950561777834,64.3380787477797,203.739764300592));
#33947=CARTESIAN_POINT('Ctrl Pts',(26.773130908755,64.0128926025622,203.716383073535));
#33948=CARTESIAN_POINT('Ctrl Pts',(26.787903481163,63.8875395652734,203.707928735967));
#33949=CARTESIAN_POINT('Ctrl Pts',(26.787903481163,63.7619809500988,203.7));
#33950=CARTESIAN_POINT('Origin',(25.187903481163,63.761980950099,212.5));
#33951=CARTESIAN_POINT('',(26.787903481163,63.7619809500992,205.1));
#33952=CARTESIAN_POINT('',(26.787903481163,63.7619809500987,205.012499998088));
#33953=CARTESIAN_POINT('',(26.787903481163,63.761980950099,212.5));
#33954=CARTESIAN_POINT('Ctrl Pts',(26.787903481163,63.761980950099,204.312499998088));
#33955=CARTESIAN_POINT('Ctrl Pts',(26.787903481163,63.948993614655,204.32430941505));
#33956=CARTESIAN_POINT('Ctrl Pts',(26.755123306838,64.1347265371673,204.337233129786));
#33957=CARTESIAN_POINT('Ctrl Pts',(26.6185841151114,64.5086708134247,204.365824836775));
#33958=CARTESIAN_POINT('Ctrl Pts',(26.5079299539111,64.6903811727074,204.381333691723));
#33959=CARTESIAN_POINT('Ctrl Pts',(26.2230593960778,64.9999409107975,204.411267578522));
#33960=CARTESIAN_POINT('Ctrl Pts',(26.051903443519,65.124906678974,204.424500000833));
#33961=CARTESIAN_POINT('Ctrl Pts',(25.6752516759775,65.2997239560201,204.451964192216));
#33962=CARTESIAN_POINT('Ctrl Pts',(25.4741356316636,65.3494933455992,204.466628903781));
#33963=CARTESIAN_POINT('Ctrl Pts',(25.0561225496804,65.370749192906,204.497109024342));
#33964=CARTESIAN_POINT('Ctrl Pts',(24.8430251954706,65.3388723881688,204.512647373086));
#33965=CARTESIAN_POINT('Ctrl Pts',(24.4503611404348,65.1964758426224,204.5412791271));
#33966=CARTESIAN_POINT('Ctrl Pts',(24.2734513304366,65.0907111272842,204.553599830484));
#33967=CARTESIAN_POINT('Ctrl Pts',(23.9663523765791,64.8160016283683,204.582143415605));
#33968=CARTESIAN_POINT('Ctrl Pts',(23.8399956290488,64.6487001291288,204.597314874515));
#33969=CARTESIAN_POINT('Ctrl Pts',(23.6562920781972,64.2711090884843,204.627856400161));
#33970=CARTESIAN_POINT('Ctrl Pts',(23.602312744704,64.0636300296916,204.642926219087));
#33971=CARTESIAN_POINT('Ctrl Pts',(23.5790579779837,63.6491950704841,204.669944657668));
#33972=CARTESIAN_POINT('Ctrl Pts',(23.6062675524499,63.4464140350528,204.683096841887));
#33973=CARTESIAN_POINT('Ctrl Pts',(23.7373782505986,63.0547812867918,204.712607621118));
#33974=CARTESIAN_POINT('Ctrl Pts',(23.8426913754904,62.8706008495669,204.72807773049));
#33975=CARTESIAN_POINT('Ctrl Pts',(24.1195338803517,62.5522599158531,204.758273440038));
#33976=CARTESIAN_POINT('Ctrl Pts',(24.2887643768129,62.421704976831,204.771937771729));
#33977=CARTESIAN_POINT('Ctrl Pts',(24.6620546848367,62.2370421258754,204.799156856689));
#33978=CARTESIAN_POINT('Ctrl Pts',(24.8613439415423,62.1823374382017,204.813688364991));
#33979=CARTESIAN_POINT('Ctrl Pts',(25.2776046399742,62.1503923374427,204.844040707585));
#33980=CARTESIAN_POINT('Ctrl Pts',(25.4908919037134,62.1765839518245,204.859592903899));
#33981=CARTESIAN_POINT('Ctrl Pts',(25.8875113204723,62.3084868737419,204.888513069704));
#33982=CARTESIAN_POINT('Ctrl Pts',(26.0678799273478,62.4100430795969,204.900877391633));
#33983=CARTESIAN_POINT('Ctrl Pts',(26.3820689377125,62.677130053086,204.929198123557));
#33984=CARTESIAN_POINT('Ctrl Pts',(26.5123522718067,62.840707990013,204.944277604926));
#33985=CARTESIAN_POINT('Ctrl Pts',(26.7056636418925,63.2129224443078,204.974829896664));
#33986=CARTESIAN_POINT('Ctrl Pts',(26.7650632553928,63.4189512320688,204.990005748706));
#33987=CARTESIAN_POINT('Ctrl Pts',(26.786106360167,63.6743697842249,205.006902035686));
#33988=CARTESIAN_POINT('Ctrl Pts',(26.787903481163,63.7181969529131,205.009735139996));
#33989=CARTESIAN_POINT('Ctrl Pts',(26.787903481163,63.7619809500983,205.012499998088));
#33990=CARTESIAN_POINT('Ctrl Pts',(26.787903481163,63.7619809500994,205.1));
#33991=CARTESIAN_POINT('Ctrl Pts',(26.787903481163,63.6264828425327,205.091443608092));
#33992=CARTESIAN_POINT('Ctrl Pts',(26.7706999926308,63.4912888178938,205.082279207797));
#33993=CARTESIAN_POINT('Ctrl Pts',(26.6832262119226,63.1546623460736,205.057832876903));
#33994=CARTESIAN_POINT('Ctrl Pts',(26.5898345245813,62.962354263357,205.042284161272));
#33995=CARTESIAN_POINT('Ctrl Pts',(26.3384511179543,62.6316035675298,205.012233000256));
#33996=CARTESIAN_POINT('Ctrl Pts',(26.1852709114922,62.494377876291,204.99798282041));
#33997=CARTESIAN_POINT('Ctrl Pts',(25.8284519347283,62.2805296451923,204.971469774332));
#33998=CARTESIAN_POINT('Ctrl Pts',(25.6265091391473,62.2086860884792,204.956981662561));
#33999=CARTESIAN_POINT('Ctrl Pts',(25.2093276052313,62.1485135740385,204.926562175713));
#34000=CARTESIAN_POINT('Ctrl Pts',(24.9984682127779,62.1595268801106,204.91118701168));
#34001=CARTESIAN_POINT('Ctrl Pts',(24.598921244267,62.2605496429551,204.88205337856));
#34002=CARTESIAN_POINT('Ctrl Pts',(24.4134797710973,62.3472573851336,204.869435654593));
#34003=CARTESIAN_POINT('Ctrl Pts',(24.0771653217686,62.5909252241362,204.841787130184));
#34004=CARTESIAN_POINT('Ctrl Pts',(23.9317316240052,62.7485189726601,204.826533179454));
#34005=CARTESIAN_POINT('Ctrl Pts',(23.7138058929658,63.1064132848272,204.795987772974));
#34006=CARTESIAN_POINT('Ctrl Pts',(23.6415075215285,63.3021772569585,204.780989853066));
#34007=CARTESIAN_POINT('Ctrl Pts',(23.5755450635552,63.7096602484942,204.752853363912));
#34008=CARTESIAN_POINT('Ctrl Pts',(23.5821993024926,63.917403894635,204.740393365596));
#34009=CARTESIAN_POINT('Ctrl Pts',(23.6753531498165,64.3252574097626,204.711242125997));
#34010=CARTESIAN_POINT('Ctrl Pts',(23.763368903889,64.5207776850988,204.695686565403));
#34011=CARTESIAN_POINT('Ctrl Pts',(24.0058931859435,64.8595213712486,204.665453654464));
#34012=CARTESIAN_POINT('Ctrl Pts',(24.1555875636601,65.0013801322246,204.651037994492));
#34013=CARTESIAN_POINT('Ctrl Pts',(24.5077604326253,65.2258319272342,204.62402474724));
#34014=CARTESIAN_POINT('Ctrl Pts',(24.7087012206303,65.3033721329043,204.609941831497));
#34015=CARTESIAN_POINT('Ctrl Pts',(25.1256954229462,65.3744585977137,204.579536004245));
#34016=CARTESIAN_POINT('Ctrl Pts',(25.3372953688337,65.3687294288271,204.564106841524));
#34017=CARTESIAN_POINT('Ctrl Pts',(25.7395774805689,65.2774997981902,204.534773770877));
#34018=CARTESIAN_POINT('Ctrl Pts',(25.926979107786,65.1954643550273,204.521909027279));
#34019=CARTESIAN_POINT('Ctrl Pts',(26.2691032021819,64.9603581408769,204.494589339689));
#34020=CARTESIAN_POINT('Ctrl Pts',(26.4184001969773,64.8064601458988,204.479427917871));
#34021=CARTESIAN_POINT('Ctrl Pts',(26.6454454746705,64.4537256532122,204.448875858578));
#34022=CARTESIAN_POINT('Ctrl Pts',(26.7227058672447,64.2593184828226,204.43378271054));
#34023=CARTESIAN_POINT('Ctrl Pts',(26.7788529607801,63.9585157996665,204.412740687797));
#34024=CARTESIAN_POINT('Ctrl Pts',(26.787903481163,63.8602506888824,204.406205506578));
#34025=CARTESIAN_POINT('Ctrl Pts',(26.787903481163,63.761980950099,204.4));
#34026=CARTESIAN_POINT('Origin',(25.187903481163,63.761980950099,212.5));
#34027=CARTESIAN_POINT('',(26.787903481163,63.7619809500994,205.8));
#34028=CARTESIAN_POINT('',(26.787903481163,63.7619809500988,205.712499998088));
#34029=CARTESIAN_POINT('',(26.787903481163,63.761980950099,212.5));
#34030=CARTESIAN_POINT('Ctrl Pts',(26.787903481163,63.7619809500983,205.012499998088));
#34031=CARTESIAN_POINT('Ctrl Pts',(26.7879034811631,63.9203754308701,205.022502242975));
#34032=CARTESIAN_POINT('Ctrl Pts',(26.764394698655,64.078097013435,205.033319086927));
#34033=CARTESIAN_POINT('Ctrl Pts',(26.6565900458734,64.4304764207694,205.059501408952));
#34034=CARTESIAN_POINT('Ctrl Pts',(26.5564917553633,64.6169004300252,205.074923070535));
#34035=CARTESIAN_POINT('Ctrl Pts',(26.2875593368092,64.9436732159463,205.105362843473));
#34036=CARTESIAN_POINT('Ctrl Pts',(26.1202033059179,65.079700803322,205.119519802533));
#34037=CARTESIAN_POINT('Ctrl Pts',(25.750203601821,65.2737935921837,205.146498947623));
#34038=CARTESIAN_POINT('Ctrl Pts',(25.5527707440558,65.3331547757878,205.160895093502));
#34039=CARTESIAN_POINT('Ctrl Pts',(25.1384330669027,65.3752362020112,205.191107215795));
#34040=CARTESIAN_POINT('Ctrl Pts',(24.9251015083622,65.3544607625124,205.206662641938));
#34041=CARTESIAN_POINT('Ctrl Pts',(24.5248014746044,65.2326268377833,205.235851186066));
#34042=CARTESIAN_POINT('Ctrl Pts',(24.3410901005411,65.1350814473227,205.248331950634));
#34043=CARTESIAN_POINT('Ctrl Pts',(24.0202528598094,64.8752302082374,205.276438146074));
#34044=CARTESIAN_POINT('Ctrl Pts',(23.8863674965984,64.7152428409624,205.291422215258));
#34045=CARTESIAN_POINT('Ctrl Pts',(23.6841475426842,64.3483194106581,205.321965183195));
#34046=CARTESIAN_POINT('Ctrl Pts',(23.6196773382549,64.1437908321096,205.337231165791));
#34047=CARTESIAN_POINT('Ctrl Pts',(23.5753843646266,63.7308116046127,205.364924696244));
#34048=CARTESIAN_POINT('Ctrl Pts',(23.5923207633707,63.5267683405508,205.377514176774));
#34049=CARTESIAN_POINT('Ctrl Pts',(23.7032532954711,63.1298976168921,205.406620059725));
#34050=CARTESIAN_POINT('Ctrl Pts',(23.7984631158282,62.9415166825513,205.421987071124));
#34051=CARTESIAN_POINT('Ctrl Pts',(24.0579518435671,62.6094589432977,205.452416275407));
#34052=CARTESIAN_POINT('Ctrl Pts',(24.2206455088039,62.4699263013444,205.466970770937));
#34053=CARTESIAN_POINT('Ctrl Pts',(24.5834595825425,62.2665954546379,205.493425963814));
#34054=CARTESIAN_POINT('Ctrl Pts',(24.7785885703373,62.2018704889865,205.507654119174));
#34055=CARTESIAN_POINT('Ctrl Pts',(25.1903750294395,62.1480495849174,205.53768021515));
#34056=CARTESIAN_POINT('Ctrl Pts',(25.4035895306318,62.162521074076,205.553227105862));
#34057=CARTESIAN_POINT('Ctrl Pts',(25.808060349869,62.2725278142357,205.582719769765));
#34058=CARTESIAN_POINT('Ctrl Pts',(25.9957351330192,62.365391979812,205.595427499058));
#34059=CARTESIAN_POINT('Ctrl Pts',(26.3241902244079,62.6168371572382,205.623280605298));
#34060=CARTESIAN_POINT('Ctrl Pts',(26.4621032687503,62.7725947548537,205.638144416858));
#34061=CARTESIAN_POINT('Ctrl Pts',(26.6753613579213,63.134792561137,205.668791404589));
#34062=CARTESIAN_POINT('Ctrl Pts',(26.7459013793187,63.3394024204981,205.684283815291));
#34063=CARTESIAN_POINT('Ctrl Pts',(26.7832934753234,63.6216637007897,205.703471215402));
#34064=CARTESIAN_POINT('Ctrl Pts',(26.787903481163,63.6918511368568,205.708071462684));
#34065=CARTESIAN_POINT('Ctrl Pts',(26.787903481163,63.7619809500986,205.712499998088));
#34066=CARTESIAN_POINT('Ctrl Pts',(26.787903481163,63.7619809500998,205.8));
#34067=CARTESIAN_POINT('Ctrl Pts',(26.787903481163,63.5970233741762,205.789583310843));
#34068=CARTESIAN_POINT('Ctrl Pts',(26.7624058873089,63.4328282096167,205.778285166423));
#34069=CARTESIAN_POINT('Ctrl Pts',(26.6479661573429,63.0745487504577,205.751488365924));
#34070=CARTESIAN_POINT('Ctrl Pts',(26.5449154109998,62.8885614447829,205.735986639542));
#34071=CARTESIAN_POINT('Ctrl Pts',(26.2775921062976,62.5729472280983,205.706310170037));
#34072=CARTESIAN_POINT('Ctrl Pts',(26.1181448497944,62.4444819806854,205.692830099796));
#34073=CARTESIAN_POINT('Ctrl Pts',(25.7515596033761,62.2495753769853,205.666099925578));
#34074=CARTESIAN_POINT('Ctrl Pts',(25.5461691738736,62.1882350393232,205.651123540093));
#34075=CARTESIAN_POINT('Ctrl Pts',(25.1276467643565,62.1496308905272,205.620606281066));
#34076=CARTESIAN_POINT('Ctrl Pts',(24.918658424567,62.1711234328677,205.605367547956));
#34077=CARTESIAN_POINT('Ctrl Pts',(24.5247831157029,62.2916763130284,205.576647473352));
#34078=CARTESIAN_POINT('Ctrl Pts',(24.3431771222327,62.3879519502523,205.564302769579));
#34079=CARTESIAN_POINT('Ctrl Pts',(24.0179167377481,62.6498417170116,205.535906585384));
#34080=CARTESIAN_POINT('Ctrl Pts',(23.879954869629,62.815956019104,205.520386991871));
#34081=CARTESIAN_POINT('Ctrl Pts',(23.6813225898408,63.1853472172947,205.489818990723));
#34082=CARTESIAN_POINT('Ctrl Pts',(23.6197340287676,63.3836006133469,205.475054331292));
#34083=CARTESIAN_POINT('Ctrl Pts',(23.5747029995119,63.7955512694772,205.447398844463));
#34084=CARTESIAN_POINT('Ctrl Pts',(23.592813039977,64.0053928116448,205.434450109941));
#34085=CARTESIAN_POINT('Ctrl Pts',(23.7093125159563,64.4087873729732,205.404729300244));
#34086=CARTESIAN_POINT('Ctrl Pts',(23.8074847528848,64.5980587590194,205.38919805411));
#34087=CARTESIAN_POINT('Ctrl Pts',(24.066806173323,64.9215175853985,205.35931795102));
#34088=CARTESIAN_POINT('Ctrl Pts',(24.2230824675475,65.0544215778394,205.345351532243));
#34089=CARTESIAN_POINT('Ctrl Pts',(24.5846647970463,65.2590333925237,205.31898615405));
#34090=CARTESIAN_POINT('Ctrl Pts',(24.7883290378769,65.325742780325,205.30413563649));
#34091=CARTESIAN_POINT('Ctrl Pts',(25.206170580613,65.3754218477422,205.273668023998));
#34092=CARTESIAN_POINT('Ctrl Pts',(25.4161852664744,65.3592991558818,205.258354453154));
#34093=CARTESIAN_POINT('Ctrl Pts',(25.813009319228,65.2487766509945,205.229419365974));
#34094=CARTESIAN_POINT('Ctrl Pts',(25.9965736972429,65.1574589524346,205.216971771321));
#34095=CARTESIAN_POINT('Ctrl Pts',(26.328652143562,64.9041968716601,205.188871830358));
#34096=CARTESIAN_POINT('Ctrl Pts',(26.47123358898,64.7412633654917,205.173384674657));
#34097=CARTESIAN_POINT('Ctrl Pts',(26.6796688485015,64.3760948031904,205.14272592289));
#34098=CARTESIAN_POINT('Ctrl Pts',(26.7463232059866,64.1789448892568,205.127846255308));
#34099=CARTESIAN_POINT('Ctrl Pts',(26.7831857238628,63.903931748119,205.109135865945));
#34100=CARTESIAN_POINT('Ctrl Pts',(26.787903481163,63.8329256088025,205.104479991009));
#34101=CARTESIAN_POINT('Ctrl Pts',(26.787903481163,63.7619809500994,205.1));
#34102=CARTESIAN_POINT('Origin',(25.187903481163,63.761980950099,212.5));
#34103=CARTESIAN_POINT('',(26.787903481163,63.7619809500991,206.5));
#34104=CARTESIAN_POINT('',(26.787903481163,63.761980950099,206.412499998088));
#34105=CARTESIAN_POINT('',(26.787903481163,63.761980950099,212.5));
#34106=CARTESIAN_POINT('Ctrl Pts',(26.787903481163,63.7619809500986,205.712499998088));
#34107=CARTESIAN_POINT('Ctrl Pts',(26.787903481163,63.8943329583833,205.720857721108));
#34108=CARTESIAN_POINT('Ctrl Pts',(26.7714895796679,64.0264035874911,205.729796099176));
#34109=CARTESIAN_POINT('Ctrl Pts',(26.6875572351756,64.3574180908798,205.753758932389));
#34110=CARTESIAN_POINT('Ctrl Pts',(26.5972506194736,64.547623366758,205.769062384064));
#34111=CARTESIAN_POINT('Ctrl Pts',(26.3466230602689,64.8855389928907,205.79953843691));
#34112=CARTESIAN_POINT('Ctrl Pts',(26.1875546066788,65.0291679766956,205.81440764554));
#34113=CARTESIAN_POINT('Ctrl Pts',(25.8304058009002,65.241321917776,205.84082572614));
#34114=CARTESIAN_POINT('Ctrl Pts',(25.6374980048513,65.3109227042223,205.854717064069));
#34115=CARTESIAN_POINT('Ctrl Pts',(25.228111480123,65.3753410156036,205.884568164831));
#34116=CARTESIAN_POINT('Ctrl Pts',(25.0151601440169,65.3665725658219,205.900095866422));
#34117=CARTESIAN_POINT('Ctrl Pts',(24.6070218134671,65.2673819279788,205.929855953024));
#34118=CARTESIAN_POINT('Ctrl Pts',(24.4156909879703,65.1787807864123,205.942852614483));
#34119=CARTESIAN_POINT('Ctrl Pts',(24.0804425802019,64.934937537628,205.970473349515));
#34120=CARTESIAN_POINT('Ctrl Pts',(23.9390334905256,64.7830516539203,205.985220131289));
#34121=CARTESIAN_POINT('Ctrl Pts',(23.7171878133876,64.4273026847945,206.015772979022));
#34122=CARTESIAN_POINT('Ctrl Pts',(23.641561420083,64.2251364785299,206.031296519329));
#34123=CARTESIAN_POINT('Ctrl Pts',(23.5757688024019,63.812753944709,206.059736211146));
#34124=CARTESIAN_POINT('Ctrl Pts',(23.5824097134815,63.6072193302805,206.0720725426));
#34125=CARTESIAN_POINT('Ctrl Pts',(23.673441865874,63.2054789145064,206.100760400662));
#34126=CARTESIAN_POINT('Ctrl Pts',(23.7585569011475,63.0134896037899,206.115987233639));
#34127=CARTESIAN_POINT('Ctrl Pts',(23.9998699983602,62.6694564915045,206.146510001817));
#34128=CARTESIAN_POINT('Ctrl Pts',(24.1551180635514,62.5216441805762,206.161504092879));
#34129=CARTESIAN_POINT('Ctrl Pts',(24.5063252799646,62.3002726608011,206.188287621796));
#34130=CARTESIAN_POINT('Ctrl Pts',(24.6969757788931,62.2256880415114,206.201703186464));
#34131=CARTESIAN_POINT('Ctrl Pts',(25.1035511492808,62.1504001046736,206.231349307222));
#34132=CARTESIAN_POINT('Ctrl Pts',(25.316073602482,62.153291142219,206.246845736101));
#34133=CARTESIAN_POINT('Ctrl Pts',(25.7278845395229,62.2412021115542,206.276873616927));
#34134=CARTESIAN_POINT('Ctrl Pts',(25.9230557098139,62.3253657306034,206.290250163416));
#34135=CARTESIAN_POINT('Ctrl Pts',(26.2652195901742,62.5613652067408,206.317627708963));
#34136=CARTESIAN_POINT('Ctrl Pts',(26.410089584138,62.7092175623087,206.332245961572));
#34137=CARTESIAN_POINT('Ctrl Pts',(26.6405135656668,63.0581766093192,206.362682792118));
#34138=CARTESIAN_POINT('Ctrl Pts',(26.7212541523886,63.2577222668339,206.378227305805));
#34139=CARTESIAN_POINT('Ctrl Pts',(26.7787804698014,63.564663052373,206.399707219712));
#34140=CARTESIAN_POINT('Ctrl Pts',(26.787903481163,63.663318335078,206.406269682285));
#34141=CARTESIAN_POINT('Ctrl Pts',(26.787903481163,63.761980950099,206.412499998088));
#34142=CARTESIAN_POINT('Ctrl Pts',(26.787903481163,63.7619809500991,206.5));
#34143=CARTESIAN_POINT('Ctrl Pts',(26.787903481163,63.5675038931425,206.487719223933));
#34144=CARTESIAN_POINT('Ctrl Pts',(26.7524551032464,63.3744595409921,206.47423653108));
#34145=CARTESIAN_POINT('Ctrl Pts',(26.6084762635081,62.9965740307621,206.44512470712));
#34146=CARTESIAN_POINT('Ctrl Pts',(26.4961791586905,62.8173669190952,206.429714027479));
#34147=CARTESIAN_POINT('Ctrl Pts',(26.2134448205049,62.5172247748368,206.400452722944));
#34148=CARTESIAN_POINT('Ctrl Pts',(26.0475956006242,62.3974101336151,206.387685883711));
#34149=CARTESIAN_POINT('Ctrl Pts',(25.6712876897652,62.222031513499,206.36024676521));
#34150=CARTESIAN_POINT('Ctrl Pts',(25.462886059874,62.1715568643892,206.345050813031));
#34151=CARTESIAN_POINT('Ctrl Pts',(25.0438888044796,62.155081948558,206.314498929825));
#34152=CARTESIAN_POINT('Ctrl Pts',(24.8373549273612,62.1871777057293,206.299439167952));
#34153=CARTESIAN_POINT('Ctrl Pts',(24.4495807953107,62.3277374308245,206.271163970823));
#34154=CARTESIAN_POINT('Ctrl Pts',(24.2718327392805,62.4342039840849,206.258780963389));
#34155=CARTESIAN_POINT('Ctrl Pts',(23.9607494916364,62.7134916629651,206.229803016088));
#34156=CARTESIAN_POINT('Ctrl Pts',(23.8324132049372,62.8857034299824,206.214249314432));
#34157=CARTESIAN_POINT('Ctrl Pts',(23.6540181241615,63.2629139046671,206.183925358617));
#34158=CARTESIAN_POINT('Ctrl Pts',(23.6028055180387,63.4630195624287,206.169422023171));
#34159=CARTESIAN_POINT('Ctrl Pts',(23.5781678571076,63.8790318357696,206.142253562835));
#34160=CARTESIAN_POINT('Ctrl Pts',(23.6078144084343,64.0911015451921,206.128490876883));
#34161=CARTESIAN_POINT('Ctrl Pts',(23.7474692652303,64.4894792931328,206.098242660748));
#34162=CARTESIAN_POINT('Ctrl Pts',(23.8552907363838,64.672063101578,206.082781924664));
#34163=CARTESIAN_POINT('Ctrl Pts',(24.1305191199193,64.979800405088,206.053314657996));
#34164=CARTESIAN_POINT('Ctrl Pts',(24.2931987402541,65.1038466447376,206.040238887358));
#34165=CARTESIAN_POINT('Ctrl Pts',(24.6647590825583,65.2888774183122,206.013145945732));
#34166=CARTESIAN_POINT('Ctrl Pts',(24.8717496356647,65.3447302249742,205.998052884568));
#34167=CARTESIAN_POINT('Ctrl Pts',(25.2906602783368,65.3721118293582,205.967507316873));
#34168=CARTESIAN_POINT('Ctrl Pts',(25.4984710074416,65.3452210672238,205.952354451209));
#34169=CARTESIAN_POINT('Ctrl Pts',(25.8892867413197,65.2145216848601,205.923857470614));
#34170=CARTESIAN_POINT('Ctrl Pts',(26.0689326881062,65.1131282902506,205.91153430439));
#34171=CARTESIAN_POINT('Ctrl Pts',(26.3871001166582,64.8424457137608,205.882841471962));
#34172=CARTESIAN_POINT('Ctrl Pts',(26.5202476112438,64.6731947633831,205.867299330404));
#34173=CARTESIAN_POINT('Ctrl Pts',(26.708726986369,64.2997320722016,205.836844381879));
#34174=CARTESIAN_POINT('Ctrl Pts',(26.7650964196516,64.1004789522881,205.822206872901));
#34175=CARTESIAN_POINT('Ctrl Pts',(26.7860341842952,63.8513374056493,205.805710804818));
#34176=CARTESIAN_POINT('Ctrl Pts',(26.787903481163,63.8066355290279,205.802819833315));
#34177=CARTESIAN_POINT('Ctrl Pts',(26.787903481163,63.7619809500998,205.8));
#34178=CARTESIAN_POINT('Origin',(25.187903481163,63.761980950099,212.5));
#34179=CARTESIAN_POINT('',(26.787903481163,63.761980950099,207.2));
#34180=CARTESIAN_POINT('',(26.787903481163,63.7619809500991,207.112499998088));
#34181=CARTESIAN_POINT('',(26.787903481163,63.761980950099,212.5));
#34182=CARTESIAN_POINT('Ctrl Pts',(26.787903481163,63.761980950099,206.412499998088));
#34183=CARTESIAN_POINT('Ctrl Pts',(26.787903481163,63.8669814833784,206.419130538761));
#34184=CARTESIAN_POINT('Ctrl Pts',(26.7775710896497,63.9719422841774,206.426135272194));
#34185=CARTESIAN_POINT('Ctrl Pts',(26.7162585214528,64.2788956428125,206.447754020456));
#34186=CARTESIAN_POINT('Ctrl Pts',(26.636403592699,64.4725410986798,206.46289366045));
#34187=CARTESIAN_POINT('Ctrl Pts',(26.404622379655,64.822474271555,206.49344148719));
#34188=CARTESIAN_POINT('Ctrl Pts',(26.2533371620173,64.9743941693603,206.50855048404));
#34189=CARTESIAN_POINT('Ctrl Pts',(25.9081985957982,65.2049896057789,206.535695229074));
#34190=CARTESIAN_POINT('Ctrl Pts',(25.7197445976187,65.2845731385076,206.54871991668));
#34191=CARTESIAN_POINT('Ctrl Pts',(25.3160393231562,65.3705995212323,206.578156759609));
#34192=CARTESIAN_POINT('Ctrl Pts',(25.1040997470756,65.3735165796787,206.593610687032));
#34193=CARTESIAN_POINT('Ctrl Pts',(24.688769231921,65.2969019717223,206.623895203762));
#34194=CARTESIAN_POINT('Ctrl Pts',(24.4897287899226,65.2171834336825,206.63772828132));
#34195=CARTESIAN_POINT('Ctrl Pts',(24.140805289395,64.9889568079691,206.664861433838));
#34196=CARTESIAN_POINT('Ctrl Pts',(23.9926525128375,64.845132739593,206.679344994215));
#34197=CARTESIAN_POINT('Ctrl Pts',(23.7540140389359,64.5030234563659,206.709648764732));
#34198=CARTESIAN_POINT('Ctrl Pts',(23.6683427684131,64.3061666030387,206.72520325117));
#34199=CARTESIAN_POINT('Ctrl Pts',(23.5804518451138,63.897386451111,206.7542211283));
#34200=CARTESIAN_POINT('Ctrl Pts',(23.5763626287985,63.6900886543587,206.766619069941));
#34201=CARTESIAN_POINT('Ctrl Pts',(23.6470998404387,63.2836673668123,206.794862594507));
#34202=CARTESIAN_POINT('Ctrl Pts',(23.7218432357729,63.0885556424707,206.809908467972));
#34203=CARTESIAN_POINT('Ctrl Pts',(23.9442727309352,62.7331715354191,206.840459560542));
#34204=CARTESIAN_POINT('Ctrl Pts',(24.0916199902306,62.5773845806502,206.855669181692));
#34205=CARTESIAN_POINT('Ctrl Pts',(24.4308048030734,62.337925159989,206.883156602892));
#34206=CARTESIAN_POINT('Ctrl Pts',(24.6172038270259,62.2535174294369,206.895886481641));
#34207=CARTESIAN_POINT('Ctrl Pts',(25.0181007102128,62.1572951481852,206.92511854604));
#34208=CARTESIAN_POINT('Ctrl Pts',(25.2293396512559,62.1488703535295,206.940521385491));
#34209=CARTESIAN_POINT('Ctrl Pts',(25.6479031546538,62.2146190616609,206.971041640947));
#34210=CARTESIAN_POINT('Ctrl Pts',(25.8506822506942,62.290052850919,206.985381621091));
#34211=CARTESIAN_POINT('Ctrl Pts',(26.2059569395127,62.5108773418095,207.012278899665));
#34212=CARTESIAN_POINT('Ctrl Pts',(26.3571003183097,62.6508431118903,207.026627849807));
#34213=CARTESIAN_POINT('Ctrl Pts',(26.6032945590545,62.9863308225324,207.056788954007));
#34214=CARTESIAN_POINT('Ctrl Pts',(26.6935320133216,63.1805488813184,207.072343282125));
#34215=CARTESIAN_POINT('Ctrl Pts',(26.7729929267595,63.5098955615491,207.096037775242));
#34216=CARTESIAN_POINT('Ctrl Pts',(26.787903481163,63.6358376355474,207.104534339709));
#34217=CARTESIAN_POINT('Ctrl Pts',(26.787903481163,63.7619809500992,207.112499998088));
#34218=CARTESIAN_POINT('Ctrl Pts',(26.787903481163,63.761980950099,207.2));
#34219=CARTESIAN_POINT('Ctrl Pts',(26.787903481163,63.7525522129429,207.19940459707));
#34220=CARTESIAN_POINT('Ctrl Pts',(26.7878201364588,63.7431204336134,207.198805963424));
#34221=CARTESIAN_POINT('Ctrl Pts',(26.783899104122,63.5214261680704,207.18466352932));
#34222=CARTESIAN_POINT('Ctrl Pts',(26.7379395030619,63.3120852737804,207.169768525869));
#34223=CARTESIAN_POINT('Ctrl Pts',(26.5686100509296,62.9270568821559,207.139281404403));
#34224=CARTESIAN_POINT('Ctrl Pts',(26.4482055279597,62.7544583317913,207.12399245716));
#34225=CARTESIAN_POINT('Ctrl Pts',(26.1515917254345,62.4686574751092,207.095130749608));
#34226=CARTESIAN_POINT('Ctrl Pts',(25.9795960393133,62.3567786095062,207.082727582365));
#34227=CARTESIAN_POINT('Ctrl Pts',(25.5928230113361,62.1993160111005,207.054525382408));
#34228=CARTESIAN_POINT('Ctrl Pts',(25.3802594249269,62.1592184000023,207.039025954233));
#34229=CARTESIAN_POINT('Ctrl Pts',(24.9601931890366,62.1649284522877,207.008396124532));
#34230=CARTESIAN_POINT('Ctrl Pts',(24.7566557848746,62.2074757222851,206.993554855479));
#34231=CARTESIAN_POINT('Ctrl Pts',(24.3752971863953,62.3681255968876,206.965747457673));
#34232=CARTESIAN_POINT('Ctrl Pts',(24.2014062596625,62.4852668188097,206.952988831481));
#34233=CARTESIAN_POINT('Ctrl Pts',(23.9053806152225,62.7822461340029,206.923442673408));
#34234=CARTESIAN_POINT('Ctrl Pts',(23.787237955169,62.9601889469858,206.907898712102));
#34235=CARTESIAN_POINT('Ctrl Pts',(23.6300151410848,63.3443378617583,206.877908515409));
#34236=CARTESIAN_POINT('Ctrl Pts',(23.5895443702116,63.5457925868411,206.863711618893));
#34237=CARTESIAN_POINT('Ctrl Pts',(23.5862946558477,63.9615614157298,206.837338300396));
#34238=CARTESIAN_POINT('Ctrl Pts',(23.6268246611896,64.1720148428447,206.822688307262));
#34239=CARTESIAN_POINT('Ctrl Pts',(23.7865399355414,64.5618837336842,206.792246036372));
#34240=CARTESIAN_POINT('Ctrl Pts',(23.902876632678,64.7378807497438,206.776890790036));
#34241=CARTESIAN_POINT('Ctrl Pts',(24.1924756760677,65.0309779785475,206.747824079897));
#34242=CARTESIAN_POINT('Ctrl Pts',(24.3613164130033,65.1468874283103,206.73527197372));
#34243=CARTESIAN_POINT('Ctrl Pts',(24.7419805000195,65.3131954482369,206.707515217375));
#34244=CARTESIAN_POINT('Ctrl Pts',(24.9515707329539,65.3586099066965,206.692232596224));
#34245=CARTESIAN_POINT('Ctrl Pts',(25.3703900120067,65.3649041147617,206.661693690459));
#34246=CARTESIAN_POINT('Ctrl Pts',(25.5756143073771,65.3279862975776,206.646729418922));
#34247=CARTESIAN_POINT('Ctrl Pts',(25.9604830027105,65.1782107334265,206.618666076554));
#34248=CARTESIAN_POINT('Ctrl Pts',(26.1364608790847,65.0669067939199,206.606153558572));
#34249=CARTESIAN_POINT('Ctrl Pts',(26.440744275318,64.7795277983336,206.576912574596));
#34250=CARTESIAN_POINT('Ctrl Pts',(26.5644684661065,64.6046341242401,206.561357666046));
#34251=CARTESIAN_POINT('Ctrl Pts',(26.7332524044497,64.2241199869409,206.531175497817));
#34252=CARTESIAN_POINT('Ctrl Pts',(26.7795746640885,64.0233289589085,206.516807176706));
#34253=CARTESIAN_POINT('Ctrl Pts',(26.7875627091774,63.8001241285047,206.50242107742));
#34254=CARTESIAN_POINT('Ctrl Pts',(26.787903481163,63.7810464245148,206.501203940586));
#34255=CARTESIAN_POINT('Ctrl Pts',(26.787903481163,63.7619809500991,206.5));
#34256=CARTESIAN_POINT('Origin',(25.187903481163,63.761980950099,212.5));
#34257=CARTESIAN_POINT('',(26.787903481163,63.7619809500987,207.9));
#34258=CARTESIAN_POINT('',(26.787903481163,63.7619809500993,207.812499998088));
#34259=CARTESIAN_POINT('',(26.787903481163,63.761980950099,212.5));
#34260=CARTESIAN_POINT('Ctrl Pts',(26.787903481163,63.7619809500992,207.112499998088));
#34261=CARTESIAN_POINT('Ctrl Pts',(26.787903481163,63.8414450419085,207.117517971582));
#34262=CARTESIAN_POINT('Ctrl Pts',(26.7819848945636,63.9209615052248,207.122755034017));
#34263=CARTESIAN_POINT('Ctrl Pts',(26.7394037831285,64.204148469419,207.142190071779));
#34264=CARTESIAN_POINT('Ctrl Pts',(26.6694314194012,64.4005037511713,207.157140529156));
#34265=CARTESIAN_POINT('Ctrl Pts',(26.4558083281594,64.7607282463888,207.187676214227));
#34266=CARTESIAN_POINT('Ctrl Pts',(26.3122128226757,64.9200152164406,207.202970070551));
#34267=CARTESIAN_POINT('Ctrl Pts',(25.9786438161088,65.1676690187884,207.230770205053));
#34268=CARTESIAN_POINT('Ctrl Pts',(25.7940990874182,65.2565620664902,207.243298235132));
#34269=CARTESIAN_POINT('Ctrl Pts',(25.395840262536,65.3621086082077,207.272337941113));
#34270=CARTESIAN_POINT('Ctrl Pts',(25.1853676245001,65.3755574371444,207.287684904303));
#34271=CARTESIAN_POINT('Ctrl Pts',(24.7677560754606,65.3203677089534,207.318135746421));
#34272=CARTESIAN_POINT('Ctrl Pts',(24.5650041381801,65.2509311543605,207.332852777124));
#34273=CARTESIAN_POINT('Ctrl Pts',(24.2059193595989,65.0414997397462,207.35916951882));
#34274=CARTESIAN_POINT('Ctrl Pts',(24.0512725597523,64.9063076011827,207.373344754072));
#34275=CARTESIAN_POINT('Ctrl Pts',(23.7961294931413,64.5790903688926,207.40330985598));
#34276=CARTESIAN_POINT('Ctrl Pts',(23.7004427116352,64.3882183961412,207.418851559899));
#34277=CARTESIAN_POINT('Ctrl Pts',(23.5897447945303,63.9836613539396,207.448434262406));
#34278=CARTESIAN_POINT('Ctrl Pts',(23.5744955769871,63.7743576134366,207.461229610602));
#34279=CARTESIAN_POINT('Ctrl Pts',(23.6246916716907,63.3634812780015,207.489005566243));
#34280=CARTESIAN_POINT('Ctrl Pts',(23.6889197287988,63.1657863788744,207.503831189512));
#34281=CARTESIAN_POINT('Ctrl Pts',(23.8926661586705,62.7985618703457,207.534448822611));
#34282=CARTESIAN_POINT('Ctrl Pts',(24.0330416160228,62.634088036499,207.549952819791));
#34283=CARTESIAN_POINT('Ctrl Pts',(24.3618619747844,62.3766815978009,207.578195682924));
#34284=CARTESIAN_POINT('Ctrl Pts',(24.5444809220034,62.282989638787,207.590583769816));
#34285=CARTESIAN_POINT('Ctrl Pts',(24.9398951216553,62.1676393644531,207.619416055207));
#34286=CARTESIAN_POINT('Ctrl Pts',(25.149432996067,62.148928426027,207.63469485855));
#34287=CARTESIAN_POINT('Ctrl Pts',(25.5676390031476,62.1932803902761,207.665189046566));
#34288=CARTESIAN_POINT('Ctrl Pts',(25.7721517899316,62.2574129880585,207.680101437269));
#34289=CARTESIAN_POINT('Ctrl Pts',(26.1361523885087,62.4573606483448,207.706643147582));
#34290=CARTESIAN_POINT('Ctrl Pts',(26.2939522590617,62.5881190747884,207.720364699034));
#34291=CARTESIAN_POINT('Ctrl Pts',(26.5563272541312,62.90679721156,207.75005424088));
#34292=CARTESIAN_POINT('Ctrl Pts',(26.6564631834237,63.0932056096546,207.765476288902));
#34293=CARTESIAN_POINT('Ctrl Pts',(26.764364701095,63.4456647291453,207.791667176098));
#34294=CARTESIAN_POINT('Ctrl Pts',(26.787903481163,63.6034854768915,207.802491375762));
#34295=CARTESIAN_POINT('Ctrl Pts',(26.787903481163,63.7619809500997,207.812499998088));
#34296=CARTESIAN_POINT('Ctrl Pts',(26.787903481163,63.7619809500984,207.9));
#34297=CARTESIAN_POINT('Ctrl Pts',(26.787903481163,63.7243079680956,207.897621038373));
#34298=CARTESIAN_POINT('Ctrl Pts',(26.7865729824725,63.6865997397188,207.895191343255));
#34299=CARTESIAN_POINT('Ctrl Pts',(26.7688988089106,63.437094806524,207.878791313244));
#34300=CARTESIAN_POINT('Ctrl Pts',(26.7118745467737,63.2304111462137,207.863660708868));
#34301=CARTESIAN_POINT('Ctrl Pts',(26.5227629248067,62.8558053002262,207.833110522096));
#34302=CARTESIAN_POINT('Ctrl Pts',(26.3941907240463,62.6905811369211,207.81798947041));
#34303=CARTESIAN_POINT('Ctrl Pts',(26.0831113321561,62.420141149911,207.789570374949));
#34304=CARTESIAN_POINT('Ctrl Pts',(25.9042701815625,62.3167301764244,207.777235071904));
#34305=CARTESIAN_POINT('Ctrl Pts',(25.5093829261866,62.1801962118329,207.748441209533));
#34306=CARTESIAN_POINT('Ctrl Pts',(25.2961612486276,62.151500057009,207.732893795544));
#34307=CARTESIAN_POINT('Ctrl Pts',(24.8790950172265,62.1787423660481,207.702482716171));
#34308=CARTESIAN_POINT('Ctrl Pts',(24.6789856363008,62.2312788529102,207.687891407145));
#34309=CARTESIAN_POINT('Ctrl Pts',(24.3042032141398,62.4115984513379,207.660563522196));
#34310=CARTESIAN_POINT('Ctrl Pts',(24.134119969933,62.539672230542,207.647100109662));
#34311=CARTESIAN_POINT('Ctrl Pts',(23.853707430182,62.8541361711949,207.617019065731));
#34312=CARTESIAN_POINT('Ctrl Pts',(23.7460247799713,63.0372425981383,207.601530388678));
#34313=CARTESIAN_POINT('Ctrl Pts',(23.6101306899241,63.4275875000795,207.571926539466));
#34314=CARTESIAN_POINT('Ctrl Pts',(23.5805037377593,63.6301046122382,207.558597467845));
#34315=CARTESIAN_POINT('Ctrl Pts',(23.5988520001172,64.0448225402752,207.531740043409));
#34316=CARTESIAN_POINT('Ctrl Pts',(23.650364647311,64.2529100046123,207.516721736352));
#34317=CARTESIAN_POINT('Ctrl Pts',(23.8296670976769,64.6328538193687,207.486192095254));
#34318=CARTESIAN_POINT('Ctrl Pts',(23.9542111062302,64.8018112950849,207.470982154704));
#34319=CARTESIAN_POINT('Ctrl Pts',(24.2580861321395,65.0799549433225,207.442339250041));
#34320=CARTESIAN_POINT('Ctrl Pts',(24.4334586852997,65.1876122169457,207.430011599698));
#34321=CARTESIAN_POINT('Ctrl Pts',(24.8243161172515,65.3346987298797,207.401511578619));
#34322=CARTESIAN_POINT('Ctrl Pts',(25.0372805304777,65.3691279381029,207.385982923488));
#34323=CARTESIAN_POINT('Ctrl Pts',(25.4559918902457,65.3526875099004,207.355451886838));
#34324=CARTESIAN_POINT('Ctrl Pts',(25.657887576413,65.30514962692,207.340730326388));
#34325=CARTESIAN_POINT('Ctrl Pts',(26.0360195067286,65.1347384234157,207.313158206469));
#34326=CARTESIAN_POINT('Ctrl Pts',(26.2080294593705,65.0122333167422,207.300091783863));
#34327=CARTESIAN_POINT('Ctrl Pts',(26.496418568369,64.7065938874235,207.27027717498));
#34328=CARTESIAN_POINT('Ctrl Pts',(26.6094271514754,64.5260291333446,207.254754824049));
#34329=CARTESIAN_POINT('Ctrl Pts',(26.7528126375547,64.1475032009327,207.225624191596));
#34330=CARTESIAN_POINT('Ctrl Pts',(26.787903481163,63.9554620586892,207.212217884233));
#34331=CARTESIAN_POINT('Ctrl Pts',(26.787903481163,63.761980950099,207.2));
#34332=CARTESIAN_POINT('Origin',(25.187903481163,63.761980950099,212.5));
#34333=CARTESIAN_POINT('',(26.787903481163,63.7619809500988,208.6));
#34334=CARTESIAN_POINT('',(26.787903481163,63.761980950099,208.512499998088));
#34335=CARTESIAN_POINT('',(26.787903481163,63.761980950099,212.5));
#34336=CARTESIAN_POINT('Ctrl Pts',(26.787903481163,63.7619809500997,207.812499998088));
#34337=CARTESIAN_POINT('Ctrl Pts',(26.787903481163,63.8056642480145,207.815258497255));
#34338=CARTESIAN_POINT('Ctrl Pts',(26.7861146165017,63.8493905931841,207.81808493378));
#34339=CARTESIAN_POINT('Ctrl Pts',(26.7651281508763,64.1047120415683,207.834973023913));
#34340=CARTESIAN_POINT('Ctrl Pts',(26.705767618042,64.3107518492307,207.85014814702));
#34341=CARTESIAN_POINT('Ctrl Pts',(26.5125252086714,64.6830060953015,207.880700437324));
#34342=CARTESIAN_POINT('Ctrl Pts',(26.3822699050941,64.8466113004039,207.895780618669));
#34343=CARTESIAN_POINT('Ctrl Pts',(26.0681320770453,65.1137536200525,207.924102979553));
#34344=CARTESIAN_POINT('Ctrl Pts',(25.8877887905821,65.2153404598777,207.936466694276));
#34345=CARTESIAN_POINT('Ctrl Pts',(25.4911978350355,65.347320003828,207.965384784785));
#34346=CARTESIAN_POINT('Ctrl Pts',(25.2779114232912,65.3735529914763,207.980936918975));
#34347=CARTESIAN_POINT('Ctrl Pts',(24.8616369885109,65.3416854977625,208.011290263177));
#34348=CARTESIAN_POINT('Ctrl Pts',(24.662333987329,65.28701655059,208.02582277368));
#34349=CARTESIAN_POINT('Ctrl Pts',(24.2890188827847,65.1024255295337,208.05304366672));
#34350=CARTESIAN_POINT('Ctrl Pts',(24.1197742346218,64.9719118257991,208.06670454222));
#34351=CARTESIAN_POINT('Ctrl Pts',(23.8428723168436,64.6536350491948,208.096898366491));
#34352=CARTESIAN_POINT('Ctrl Pts',(23.737519834635,64.4694721685266,208.11236880211));
#34353=CARTESIAN_POINT('Ctrl Pts',(23.6063298640587,64.0778606163386,208.141881132998));
#34354=CARTESIAN_POINT('Ctrl Pts',(23.5790801805219,63.8750840617643,208.155036115506));
#34355=CARTESIAN_POINT('Ctrl Pts',(23.6022533838314,63.4606442276958,208.182051888257));
#34356=CARTESIAN_POINT('Ctrl Pts',(23.6561917661913,63.2531548067158,208.197120868521));
#34357=CARTESIAN_POINT('Ctrl Pts',(23.8398223974902,62.8755242290384,208.227662232314));
#34358=CARTESIAN_POINT('Ctrl Pts',(23.9661491818328,62.7081950422413,208.242834347222));
#34359=CARTESIAN_POINT('Ctrl Pts',(24.2731946119985,62.4334283554682,208.271379592238));
#34360=CARTESIAN_POINT('Ctrl Pts',(24.4500787049065,62.3276321216025,208.283700274819));
#34361=CARTESIAN_POINT('Ctrl Pts',(24.8427128071976,62.1851572893188,208.312329844778));
#34362=CARTESIAN_POINT('Ctrl Pts',(25.055808187246,62.15323793446,208.327868049573));
#34363=CARTESIAN_POINT('Ctrl Pts',(25.473833358999,62.1744135890098,208.35834905168));
#34364=CARTESIAN_POINT('Ctrl Pts',(25.674962606062,62.2241458580207,208.373014725945));
#34365=CARTESIAN_POINT('Ctrl Pts',(26.0516391923357,62.3988896184487,208.400480727028));
#34366=CARTESIAN_POINT('Ctrl Pts',(26.2228094273173,62.5238141254902,208.413710241233));
#34367=CARTESIAN_POINT('Ctrl Pts',(26.5077390647548,62.8333084000493,208.443642148105));
#34368=CARTESIAN_POINT('Ctrl Pts',(26.6184326947677,63.0149998441212,208.459151247569));
#34369=CARTESIAN_POINT('Ctrl Pts',(26.7550853208744,63.3890216421474,208.487751985506));
#34370=CARTESIAN_POINT('Ctrl Pts',(26.787903481163,63.5748601181481,208.500683750606));
#34371=CARTESIAN_POINT('Ctrl Pts',(26.787903481163,63.761980950099,208.512499998088));
#34372=CARTESIAN_POINT('Ctrl Pts',(26.787903481163,63.7619809500986,208.6));
#34373=CARTESIAN_POINT('Ctrl Pts',(26.787903481163,63.6903170416566,208.595474590034));
#34374=CARTESIAN_POINT('Ctrl Pts',(26.7830895983552,63.6185920864977,208.590769818965));
#34375=CARTESIAN_POINT('Ctrl Pts',(26.7457547260124,63.3428845494794,208.571998358854));
#34376=CARTESIAN_POINT('Ctrl Pts',(26.6788199082709,63.145799591795,208.557112567994));
#34377=CARTESIAN_POINT('Ctrl Pts',(26.4698434177921,62.7808726668203,208.526449342687));
#34378=CARTESIAN_POINT('Ctrl Pts',(26.3270077628508,62.6181192181451,208.510964289145));
#34379=CARTESIAN_POINT('Ctrl Pts',(25.9945535381211,62.3653376727936,208.482880992627));
#34380=CARTESIAN_POINT('Ctrl Pts',(25.8108789472433,62.2742944396459,208.470425294402));
#34381=CARTESIAN_POINT('Ctrl Pts',(25.4138922132662,62.1643328958762,208.441478345049));
#34382=CARTESIAN_POINT('Ctrl Pts',(25.2038241981467,62.1485113437469,208.426160885613));
#34383=CARTESIAN_POINT('Ctrl Pts',(24.7860294148133,62.1988088945462,208.395696682662));
#34384=CARTESIAN_POINT('Ctrl Pts',(24.5824658822676,62.2658167581286,208.380853508414));
#34385=CARTESIAN_POINT('Ctrl Pts',(24.2211657629679,62.4709696707996,208.354508708048));
#34386=CARTESIAN_POINT('Ctrl Pts',(24.0650662140339,62.6041240979823,208.340512538584));
#34387=CARTESIAN_POINT('Ctrl Pts',(23.807380615723,62.9265435585416,208.310757708387));
#34388=CARTESIAN_POINT('Ctrl Pts',(23.7100510270448,63.1140930482654,208.295365917533));
#34389=CARTESIAN_POINT('Ctrl Pts',(23.5949105617204,63.5098968986751,208.266173990926));
#34390=CARTESIAN_POINT('Ctrl Pts',(23.575820026113,63.7136565425895,208.253492117129));
#34391=CARTESIAN_POINT('Ctrl Pts',(23.6156799993393,64.1269759559357,208.225938724534));
#34392=CARTESIAN_POINT('Ctrl Pts',(23.6779527268435,64.3321719207942,208.210710714382));
#34393=CARTESIAN_POINT('Ctrl Pts',(23.8763213986302,64.7014197159999,208.180161379509));
#34394=CARTESIAN_POINT('Ctrl Pts',(24.0086542364851,64.8629760269156,208.165134837652));
#34395=CARTESIAN_POINT('Ctrl Pts',(24.3266082436035,65.1259766875288,208.136934881423));
#34396=CARTESIAN_POINT('Ctrl Pts',(24.5088567403975,65.2252694358942,208.124513824847));
#34397=CARTESIAN_POINT('Ctrl Pts',(24.9075646962965,65.3514986296844,208.09544136973));
#34398=CARTESIAN_POINT('Ctrl Pts',(25.1208933792387,65.3746331094214,208.079886153265));
#34399=CARTESIAN_POINT('Ctrl Pts',(25.5360991086036,65.3369609364821,208.049610735499));
#34400=CARTESIAN_POINT('Ctrl Pts',(25.7343544727492,65.2796224664386,208.035154615197));
#34401=CARTESIAN_POINT('Ctrl Pts',(26.1057984283124,65.0896437082546,208.008070160104));
#34402=CARTESIAN_POINT('Ctrl Pts',(26.2739765223907,64.9560181854706,207.994137608416));
#34403=CARTESIAN_POINT('Ctrl Pts',(26.5463869939338,64.6329260627183,207.963803456824));
#34404=CARTESIAN_POINT('Ctrl Pts',(26.6487719530388,64.4474657572087,207.948359282776));
#34405=CARTESIAN_POINT('Ctrl Pts',(26.7625332992819,64.0902789679199,207.921656214591));
#34406=CARTESIAN_POINT('Ctrl Pts',(26.7879034811631,63.9265241416833,207.910390521745));
#34407=CARTESIAN_POINT('Ctrl Pts',(26.787903481163,63.7619809500984,207.9));
#34408=CARTESIAN_POINT('Origin',(25.187903481163,63.761980950099,212.5));
#34409=CARTESIAN_POINT('',(26.787903481163,63.761980950099,209.3));
#34410=CARTESIAN_POINT('',(26.787903481163,63.761980950099,209.212499998088));
#34411=CARTESIAN_POINT('',(26.787903481163,63.761980950099,212.5));
#34412=CARTESIAN_POINT('Ctrl Pts',(26.787903481163,63.7619809500991,208.512499998088));
#34413=CARTESIAN_POINT('Ctrl Pts',(26.787903481163,63.7775474145994,208.513482984296));
#34414=CARTESIAN_POINT('Ctrl Pts',(26.7876763117769,63.7931217265644,208.51447474827));
#34415=CARTESIAN_POINT('Ctrl Pts',(26.781022091544,64.0209184771424,208.529102187656));
#34416=CARTESIAN_POINT('Ctrl Pts',(26.7326473328888,64.229733878515,208.544052060066));
#34417=CARTESIAN_POINT('Ctrl Pts',(26.5589693241796,64.61258673282,208.57456034251));
#34418=CARTESIAN_POINT('Ctrl Pts',(26.4367544896036,64.7836163848673,208.589816218399));
#34419=CARTESIAN_POINT('Ctrl Pts',(26.1369815391396,65.066098938011,208.618583560031));
#34420=CARTESIAN_POINT('Ctrl Pts',(25.9635309531092,65.1761477348963,208.630943828259));
#34421=CARTESIAN_POINT('Ctrl Pts',(25.5749786481579,65.3291274817817,208.659275767161));
#34422=CARTESIAN_POINT('Ctrl Pts',(25.3622237844917,65.3667728207009,208.674789142637));
#34423=CARTESIAN_POINT('Ctrl Pts',(24.9427105504864,65.3564144508637,208.705378649283));
#34424=CARTESIAN_POINT('Ctrl Pts',(24.7398682029649,65.3117022399689,208.720169237123));
#34425=CARTESIAN_POINT('Ctrl Pts',(24.3598955373424,65.1468328837485,208.747875577325));
#34426=CARTESIAN_POINT('Ctrl Pts',(24.1868162294044,65.0273876946373,208.760757130098));
#34427=CARTESIAN_POINT('Ctrl Pts',(23.8940651100409,64.7266694324474,208.790420010294));
#34428=CARTESIAN_POINT('Ctrl Pts',(23.7781276598159,64.5475793782385,208.805956018954));
#34429=CARTESIAN_POINT('Ctrl Pts',(23.6253804438905,64.1619200072396,208.835878424612));
#34430=CARTESIAN_POINT('Ctrl Pts',(23.5872736285872,63.9602324372348,208.849957912115));
#34431=CARTESIAN_POINT('Ctrl Pts',(23.5885773167067,63.5446904835471,208.876245955095));
#34432=CARTESIAN_POINT('Ctrl Pts',(23.6314779189152,63.3347270515375,208.891068744362));
#34433=CARTESIAN_POINT('Ctrl Pts',(23.7952752504989,62.9470217655082,208.921523213619));
#34434=CARTESIAN_POINT('Ctrl Pts',(23.913364966278,62.7724682616747,208.936851217637));
#34435=CARTESIAN_POINT('Ctrl Pts',(24.20597348562,62.482489234716,208.965830741023));
#34436=CARTESIAN_POINT('Ctrl Pts',(24.3761552541167,62.3683036891449,208.978310023199));
#34437=CARTESIAN_POINT('Ctrl Pts',(24.7606685283092,62.2052260923822,209.006347449443));
#34438=CARTESIAN_POINT('Ctrl Pts',(24.9729534744288,62.1620508183978,209.021826560097));
#34439=CARTESIAN_POINT('Ctrl Pts',(25.3936421928073,62.161913910055,209.052501779146));
#34440=CARTESIAN_POINT('Ctrl Pts',(25.5980191227873,62.2017314157506,209.067404263623));
#34441=CARTESIAN_POINT('Ctrl Pts',(25.9810962854264,62.3570914833136,209.095336973399));
#34442=CARTESIAN_POINT('Ctrl Pts',(26.1560028163382,62.4713752998897,209.107963193064));
#34443=CARTESIAN_POINT('Ctrl Pts',(26.4560776856708,62.7636778317421,209.137361651083));
#34444=CARTESIAN_POINT('Ctrl Pts',(26.5769540073409,62.9401536355283,209.152912638901));
#34445=CARTESIAN_POINT('Ctrl Pts',(26.739829675257,63.3225711041239,209.182999592404));
#34446=CARTESIAN_POINT('Ctrl Pts',(26.7831573581791,63.5237230098691,209.197281524831));
#34447=CARTESIAN_POINT('Ctrl Pts',(26.7877807320592,63.7390911262713,209.21105008346));
#34448=CARTESIAN_POINT('Ctrl Pts',(26.787903481163,63.7505383731459,209.211777425835));
#34449=CARTESIAN_POINT('Ctrl Pts',(26.787903481163,63.761980950099,209.212499998088));
#34450=CARTESIAN_POINT('Ctrl Pts',(26.787903481163,63.761980950099,209.3));
#34451=CARTESIAN_POINT('Ctrl Pts',(26.787903481163,63.6629707403392,209.293747734394));
#34452=CARTESIAN_POINT('Ctrl Pts',(26.7787160838662,63.5639686077502,209.287161021649));
#34453=CARTESIAN_POINT('Ctrl Pts',(26.7220086825207,63.2624852334651,209.266055586947));
#34454=CARTESIAN_POINT('Ctrl Pts',(26.6444624854735,63.0681602008647,209.250957205766));
#34455=CARTESIAN_POINT('Ctrl Pts',(26.416894414014,62.7157307945329,209.220405351781));
#34456=CARTESIAN_POINT('Ctrl Pts',(26.267377327109,62.5620491563593,209.205249568203));
#34457=CARTESIAN_POINT('Ctrl Pts',(25.9249204273251,62.3274386412541,209.17794904933));
#34458=CARTESIAN_POINT('Ctrl Pts',(25.7374038321486,62.2456729341707,209.165067733926));
#34459=CARTESIAN_POINT('Ctrl Pts',(25.3349647129544,62.155013595733,209.135723214818));
#34460=CARTESIAN_POINT('Ctrl Pts',(25.1233257200401,62.1495925231142,209.120291204918));
#34461=CARTESIAN_POINT('Ctrl Pts',(24.7065124792662,62.2212866237006,209.089898572778));
#34462=CARTESIAN_POINT('Ctrl Pts',(24.5057807588094,62.2990664084693,209.075843943418));
#34463=CARTESIAN_POINT('Ctrl Pts',(24.1539632003856,62.523932209519,209.048817506672));
#34464=CARTESIAN_POINT('Ctrl Pts',(24.0044362203571,62.6660067634534,209.034394322915));
#34465=CARTESIAN_POINT('Ctrl Pts',(23.7623348024638,63.0051207377533,209.004153446058));
#34466=CARTESIAN_POINT('Ctrl Pts',(23.6745745699214,63.2007885440448,208.988597885115));
#34467=CARTESIAN_POINT('Ctrl Pts',(23.5819964353755,63.6087447977246,208.959461147342));
#34468=CARTESIAN_POINT('Ctrl Pts',(23.5756230379735,63.8164391368395,208.947008816032));
#34469=CARTESIAN_POINT('Ctrl Pts',(23.6421067655174,64.2238069935368,208.918860592756));
#34470=CARTESIAN_POINT('Ctrl Pts',(23.7146720858874,64.4195012863386,208.903857340423));
#34471=CARTESIAN_POINT('Ctrl Pts',(23.9330904916492,64.7771245699987,208.873311086667));
#34472=CARTESIAN_POINT('Ctrl Pts',(24.0787340467908,64.9345223966226,208.858061856901));
#34473=CARTESIAN_POINT('Ctrl Pts',(24.4153626413047,65.1777316983955,208.830430834847));
#34474=CARTESIAN_POINT('Ctrl Pts',(24.6009079018128,65.2641884922171,208.817801760994));
#34475=CARTESIAN_POINT('Ctrl Pts',(25.0006024605227,65.3646894300876,208.788657366088));
#34476=CARTESIAN_POINT('Ctrl Pts',(25.2115046509785,65.3754215440957,208.773279081368));
#34477=CARTESIAN_POINT('Ctrl Pts',(25.6286330721951,65.3146747893705,208.742863467321));
#34478=CARTESIAN_POINT('Ctrl Pts',(25.8304808168065,65.2425542867193,208.728400814344));
#34479=CARTESIAN_POINT('Ctrl Pts',(26.1870350588532,65.0281984522,208.701865366071));
#34480=CARTESIAN_POINT('Ctrl Pts',(26.3400444864997,64.8907393312025,208.687606671987));
#34481=CARTESIAN_POINT('Ctrl Pts',(26.5909913895424,64.5595839971385,208.657545873196));
#34482=CARTESIAN_POINT('Ctrl Pts',(26.6841171531266,64.3671120691719,208.641996506253));
#34483=CARTESIAN_POINT('Ctrl Pts',(26.7709008326391,64.0310957604075,208.617613865684));
#34484=CARTESIAN_POINT('Ctrl Pts',(26.787903481163,63.8966856473105,208.608506289881));
#34485=CARTESIAN_POINT('Ctrl Pts',(26.787903481163,63.7619809500986,208.6));
#34486=CARTESIAN_POINT('Origin',(25.187903481163,63.761980950099,212.5));
#34487=CARTESIAN_POINT('',(26.787903481163,63.7619809500991,210.));
#34488=CARTESIAN_POINT('',(26.787903481163,63.7619809500987,209.912499998088));
#34489=CARTESIAN_POINT('',(26.787903481163,63.761980950099,212.5));
#34490=CARTESIAN_POINT('Ctrl Pts',(26.787903481163,63.761980950099,209.212499998088));
#34491=CARTESIAN_POINT('Ctrl Pts',(26.787903481163,63.9625096575748,209.22516292188));
#34492=CARTESIAN_POINT('Ctrl Pts',(26.7502103395188,64.1614336463926,209.239098740525));
#34493=CARTESIAN_POINT('Ctrl Pts',(26.5998957155974,64.5430426346555,209.268676685637));
#34494=CARTESIAN_POINT('Ctrl Pts',(26.4857614108062,64.7208094997246,209.284063398288));
#34495=CARTESIAN_POINT('Ctrl Pts',(26.1999165351698,65.0177711203375,209.313237265127));
#34496=CARTESIAN_POINT('Ctrl Pts',(26.0327231649848,65.1358206933445,209.325898562809));
#34497=CARTESIAN_POINT('Ctrl Pts',(25.6544426944634,65.3071185037487,209.353481513785));
#34498=CARTESIAN_POINT('Ctrl Pts',(25.4454898692234,65.3553169153305,209.368717657292));
#34499=CARTESIAN_POINT('Ctrl Pts',(25.0265418719815,65.3672025982405,209.399265948758));
#34500=CARTESIAN_POINT('Ctrl Pts',(24.8205842473973,65.3329288175183,209.414283692217));
#34501=CARTESIAN_POINT('Ctrl Pts',(24.4341113143586,65.1882168295297,209.442464010251));
#34502=CARTESIAN_POINT('Ctrl Pts',(24.2571614818908,65.0795829150789,209.454896452059));
#34503=CARTESIAN_POINT('Ctrl Pts',(23.9491198501745,64.7966550553686,209.483993376107));
#34504=CARTESIAN_POINT('Ctrl Pts',(23.8228479130678,64.6232243222286,209.499548789907));
#34505=CARTESIAN_POINT('Ctrl Pts',(23.6487613566745,64.2445008384581,209.529811207126));
#34506=CARTESIAN_POINT('Ctrl Pts',(23.5997439461575,64.0440727594058,209.544254869558));
#34507=CARTESIAN_POINT('Ctrl Pts',(23.5794462759211,63.6272334648883,209.57131732554));
#34508=CARTESIAN_POINT('Ctrl Pts',(23.6116007681108,63.4146720776778,209.585295713189));
#34509=CARTESIAN_POINT('Ctrl Pts',(23.7562325183374,63.017454396937,209.615652123004));
#34510=CARTESIAN_POINT('Ctrl Pts',(23.8660690515765,62.8363682030017,209.631091754003));
#34511=CARTESIAN_POINT('Ctrl Pts',(24.1446650021707,62.532024541803,209.660467495895));
#34512=CARTESIAN_POINT('Ctrl Pts',(24.3087540644221,62.409872210698,209.673395353117));
#34513=CARTESIAN_POINT('Ctrl Pts',(24.6824419683471,62.229138169489,209.700643429445));
#34514=CARTESIAN_POINT('Ctrl Pts',(24.8900793264089,62.1756781715759,209.715783653471));
#34515=CARTESIAN_POINT('Ctrl Pts',(25.3090639956147,62.1531602042708,209.746334618934));
#34516=CARTESIAN_POINT('Ctrl Pts',(25.5163214487618,62.1823770473555,209.761447141559));
#34517=CARTESIAN_POINT('Ctrl Pts',(25.9057883099507,62.3174722790651,209.789845766854));
#34518=CARTESIAN_POINT('Ctrl Pts',(26.084589526411,62.4211161840766,209.802185836687));
#34519=CARTESIAN_POINT('Ctrl Pts',(26.3996213423553,62.6956275303874,209.831006127859));
#34520=CARTESIAN_POINT('Ctrl Pts',(26.5306397132082,62.8662097222909,209.846554709935));
#34521=CARTESIAN_POINT('Ctrl Pts',(26.7146489611726,63.2413697020022,209.876953864917));
#34522=CARTESIAN_POINT('Ctrl Pts',(26.7687292090268,63.4410177911385,209.891532855402));
#34523=CARTESIAN_POINT('Ctrl Pts',(26.7864907564276,63.6843022602055,209.907543263004));
#34524=CARTESIAN_POINT('Ctrl Pts',(26.787903481163,63.7231612765527,209.910048625544));
#34525=CARTESIAN_POINT('Ctrl Pts',(26.787903481163,63.7619809500983,209.912499998088));
#34526=CARTESIAN_POINT('Ctrl Pts',(26.787903481163,63.7619809500992,210.));
#34527=CARTESIAN_POINT('Ctrl Pts',(26.787903481163,63.635661259033,209.992023203852));
#34528=CARTESIAN_POINT('Ctrl Pts',(26.7729513315449,63.5095551023203,209.983514761449));
#34529=CARTESIAN_POINT('Ctrl Pts',(26.6942281251588,63.1837109674741,209.960068341537));
#34530=CARTESIAN_POINT('Ctrl Pts',(26.606212810655,62.9926997944486,209.944797536345));
#34531=CARTESIAN_POINT('Ctrl Pts',(26.3596846196389,62.6520478145269,209.914298145222));
#34532=CARTESIAN_POINT('Ctrl Pts',(26.2022910462423,62.5065565628155,209.899372402024));
#34533=CARTESIAN_POINT('Ctrl Pts',(25.8477593079741,62.2903196808869,209.872791907078));
#34534=CARTESIAN_POINT('Ctrl Pts',(25.6558592320014,62.2185120888091,209.859121773499));
#34535=CARTESIAN_POINT('Ctrl Pts',(25.2477105958396,62.1492614922979,209.829360935445));
#34536=CARTESIAN_POINT('Ctrl Pts',(25.0349300186893,62.1554178305597,209.813845685028));
#34537=CARTESIAN_POINT('Ctrl Pts',(24.6251458927997,62.2496130926411,209.783965592515));
#34538=CARTESIAN_POINT('Ctrl Pts',(24.4321175076648,62.3362485402014,209.770810338485));
#34539=CARTESIAN_POINT('Ctrl Pts',(24.093785600076,62.5766076676862,209.743297198385));
#34540=CARTESIAN_POINT('Ctrl Pts',(23.9508208408974,62.7267062961762,209.728606560525));
#34541=CARTESIAN_POINT('Ctrl Pts',(23.725129139662,63.0794554025556,209.698102927553));
#34542=CARTESIAN_POINT('Ctrl Pts',(23.6472140844721,63.2804695810034,209.682568694339));
#34543=CARTESIAN_POINT('Ctrl Pts',(23.5764456589093,63.6920806143508,209.653996311329));
#34544=CARTESIAN_POINT('Ctrl Pts',(23.5806743473847,63.8979958834204,209.64167453391));
#34545=CARTESIAN_POINT('Ctrl Pts',(23.667100980843,64.3008226245383,209.613085986462));
#34546=CARTESIAN_POINT('Ctrl Pts',(23.7498671504022,64.4935701194035,209.59789691164));
#34547=CARTESIAN_POINT('Ctrl Pts',(23.986935465546,64.8402746188052,209.567360209227));
#34548=CARTESIAN_POINT('Ctrl Pts',(24.1404252825187,64.9899373162383,209.552313373339));
#34549=CARTESIAN_POINT('Ctrl Pts',(24.4889292317419,65.2154412930024,209.525367445943));
#34550=CARTESIAN_POINT('Ctrl Pts',(24.6785881192932,65.2922634592259,209.51213757847));
#34551=CARTESIAN_POINT('Ctrl Pts',(25.0838844226146,65.3723790789397,209.482584723019));
#34552=CARTESIAN_POINT('Ctrl Pts',(25.2961645249118,65.3720995389519,209.46710596556));
#34553=CARTESIAN_POINT('Ctrl Pts',(25.7095716663637,65.2892482902382,209.436961694829));
#34554=CARTESIAN_POINT('Ctrl Pts',(25.9064733534398,65.2070749914989,209.423389817729));
#34555=CARTESIAN_POINT('Ctrl Pts',(26.2516850693628,64.9745670252063,209.396121633943));
#34556=CARTESIAN_POINT('Ctrl Pts',(26.3980477416357,64.8285207487543,209.381563010488));
#34557=CARTESIAN_POINT('Ctrl Pts',(26.6321970240694,64.4826245370138,209.351183772638));
#34558=CARTESIAN_POINT('Ctrl Pts',(26.7151695069104,64.2842757963881,209.33563347027));
#34559=CARTESIAN_POINT('Ctrl Pts',(26.777564314995,63.9720117850579,209.313639909918));
#34560=CARTESIAN_POINT('Ctrl Pts',(26.787903481163,63.8670158574599,209.306632711317));
#34561=CARTESIAN_POINT('Ctrl Pts',(26.787903481163,63.761980950099,209.3));
#34562=CARTESIAN_POINT('Origin',(25.187903481163,63.761980950099,212.5));
#34563=CARTESIAN_POINT('',(26.787903481163,63.7619809500994,210.7));
#34564=CARTESIAN_POINT('',(26.787903481163,63.7619809500987,210.612499998088));
#34565=CARTESIAN_POINT('',(26.787903481163,63.761980950099,212.5));
#34566=CARTESIAN_POINT('Ctrl Pts',(26.787903481163,63.7619809500983,209.912499998088));
#34567=CARTESIAN_POINT('Ctrl Pts',(26.7879034811631,63.9335970442676,209.923337157262));
#34568=CARTESIAN_POINT('Ctrl Pts',(26.7603050063469,64.1043181033942,209.93512399144));
#34569=CARTESIAN_POINT('Ctrl Pts',(26.6394171169629,64.4672093546526,209.962447105082));
#34570=CARTESIAN_POINT('Ctrl Pts',(26.534242295437,64.6517055105942,209.97793210905));
#34571=CARTESIAN_POINT('Ctrl Pts',(26.2634103644491,64.9638391022234,210.007516703806));
#34572=CARTESIAN_POINT('Ctrl Pts',(26.1025412418608,65.0903474203494,210.020807661371));
#34573=CARTESIAN_POINT('Ctrl Pts',(25.7337514358277,65.2809066557851,210.047698584727));
#34574=CARTESIAN_POINT('Ctrl Pts',(25.5276371511831,65.339833831516,210.062727751316));
#34575=CARTESIAN_POINT('Ctrl Pts',(25.1089062067284,65.3734909493857,210.093260216016));
#34576=CARTESIAN_POINT('Ctrl Pts',(24.9004199290461,65.3496134728875,210.10846234043));
#34577=CARTESIAN_POINT('Ctrl Pts',(24.5078841996179,65.2245866177153,210.137084737367));
#34578=CARTESIAN_POINT('Ctrl Pts',(24.3271448115197,65.1260675356885,210.149409580288));
#34579=CARTESIAN_POINT('Ctrl Pts',(24.0049872090873,64.8603085050649,210.177936977279));
#34580=CARTESIAN_POINT('Ctrl Pts',(23.869130810807,64.6928005525691,210.193467814668));
#34581=CARTESIAN_POINT('Ctrl Pts',(23.6749465000499,64.32158831826,210.223988644495));
#34582=CARTESIAN_POINT('Ctrl Pts',(23.615647832192,64.1228792481685,210.238698592997));
#34583=CARTESIAN_POINT('Ctrl Pts',(23.5751036531259,63.7100102747399,210.266248486358));
#34584=CARTESIAN_POINT('Ctrl Pts',(23.5957181798156,63.4996920144276,210.279347848247));
#34585=CARTESIAN_POINT('Ctrl Pts',(23.7172785329909,63.0973418160769,210.309187219987));
#34586=CARTESIAN_POINT('Ctrl Pts',(23.8175972209408,62.9094916850686,210.324706973182));
#34587=CARTESIAN_POINT('Ctrl Pts',(24.0804303953468,62.5894595343949,210.354498722328));
#34588=CARTESIAN_POINT('Ctrl Pts',(24.2380864280138,62.4584995642421,210.368242504629));
#34589=CARTESIAN_POINT('Ctrl Pts',(24.6018598470313,62.2581116168253,210.394767649766));
#34590=CARTESIAN_POINT('Ctrl Pts',(24.8062940313073,62.1937354835571,210.409674309036));
#34591=CARTESIAN_POINT('Ctrl Pts',(25.2244685855717,62.1488809917243,210.440166203618));
#34592=CARTESIAN_POINT('Ctrl Pts',(25.4340527763025,62.1673481920154,210.455448384192));
#34593=CARTESIAN_POINT('Ctrl Pts',(25.8296006406912,62.2822433160495,210.48429041597));
#34594=CARTESIAN_POINT('Ctrl Pts',(26.0123084898772,62.3757104938337,210.496683326307));
#34595=CARTESIAN_POINT('Ctrl Pts',(26.3414378648629,62.6327255493329,210.524912740713));
#34596=CARTESIAN_POINT('Ctrl Pts',(26.4820226865197,62.797054890118,210.540415246564));
#34597=CARTESIAN_POINT('Ctrl Pts',(26.6862135177991,63.1640874037339,210.571036957764));
#34598=CARTESIAN_POINT('Ctrl Pts',(26.7506712760385,63.3617320086207,210.585867779588));
#34599=CARTESIAN_POINT('Ctrl Pts',(26.7839044580146,63.6312850583613,210.604101057276));
#34600=CARTESIAN_POINT('Ctrl Pts',(26.787903481163,63.6966644992972,210.608375415382));
#34601=CARTESIAN_POINT('Ctrl Pts',(26.787903481163,63.7619809500984,210.612499998088));
#34602=CARTESIAN_POINT('Ctrl Pts',(26.787903481163,63.7619809500997,210.7));
#34603=CARTESIAN_POINT('Ctrl Pts',(26.787903481163,63.6098599431785,210.690393910468));
#34604=CARTESIAN_POINT('Ctrl Pts',(26.7662204259159,63.4583029385245,210.680032908317));
#34605=CARTESIAN_POINT('Ctrl Pts',(26.664368656578,63.1109236989383,210.654383367523));
#34606=CARTESIAN_POINT('Ctrl Pts',(26.5666136050719,62.9235442379033,210.638986801959));
#34607=CARTESIAN_POINT('Ctrl Pts',(26.3012618617114,62.593025913473,210.608441052382));
#34608=CARTESIAN_POINT('Ctrl Pts',(26.134749550499,62.4545324444443,210.594040859222));
#34609=CARTESIAN_POINT('Ctrl Pts',(25.7662324440654,62.256255964826,210.567169820212));
#34610=CARTESIAN_POINT('Ctrl Pts',(25.569655691065,62.1948521984884,210.552836098639));
#34611=CARTESIAN_POINT('Ctrl Pts',(25.1562464175635,62.1483084122457,210.522691672446));
#34612=CARTESIAN_POINT('Ctrl Pts',(24.9429378720832,62.1666916011874,210.507137924338));
#34613=CARTESIAN_POINT('Ctrl Pts',(24.5410407365537,62.2840519395233,210.477832924872));
#34614=CARTESIAN_POINT('Ctrl Pts',(24.355834723001,62.3798235040937,210.46527753717));
#34615=CARTESIAN_POINT('Ctrl Pts',(24.0320922328871,62.6364834962525,210.437266941037));
#34616=CARTESIAN_POINT('Ctrl Pts',(23.8966578737162,62.7948720268811,210.422327360876));
#34617=CARTESIAN_POINT('Ctrl Pts',(23.6905773432696,63.1594076509547,210.39179442719));
#34618=CARTESIAN_POINT('Ctrl Pts',(23.6238959356232,63.3632377791808,210.376491933331));
#34619=CARTESIAN_POINT('Ctrl Pts',(23.5751260975114,63.7758548244946,210.348658054828));
#34620=CARTESIAN_POINT('Ctrl Pts',(23.58989155688,63.9801940249824,210.336147867406));
#34621=CARTESIAN_POINT('Ctrl Pts',(23.6965976329302,64.3781231113291,210.307129240844));
#34622=CARTESIAN_POINT('Ctrl Pts',(23.7896725171562,64.5673152440865,210.291788840355));
#34623=CARTESIAN_POINT('Ctrl Pts',(24.0453559413064,64.9020147242601,210.261331551274));
#34624=CARTESIAN_POINT('Ctrl Pts',(24.2064884219356,65.0433065986533,210.246561514735));
#34625=CARTESIAN_POINT('Ctrl Pts',(24.5667970441878,65.2504923103573,210.220289011029));
#34626=CARTESIAN_POINT('Ctrl Pts',(24.7609675184813,65.3173319874089,210.206130747279));
#34627=CARTESIAN_POINT('Ctrl Pts',(25.1716461741282,65.3758005468082,210.176185428638));
#34628=CARTESIAN_POINT('Ctrl Pts',(25.3847635454736,65.3638342065162,210.160645620311));
#34629=CARTESIAN_POINT('Ctrl Pts',(25.7908578316024,65.2585640109584,210.131034578614));
#34630=CARTESIAN_POINT('Ctrl Pts',(25.9801301897951,65.1675682217721,210.11820965116));
#34631=CARTESIAN_POINT('Ctrl Pts',(26.311580130965,64.9194619400752,210.090458201226));
#34632=CARTESIAN_POINT('Ctrl Pts',(26.4510458637665,64.765399864603,210.075644849532));
#34633=CARTESIAN_POINT('Ctrl Pts',(26.668108721095,64.4060176157923,210.045036942234));
#34634=CARTESIAN_POINT('Ctrl Pts',(26.7408983027634,64.2024689537162,210.029529528466));
#34635=CARTESIAN_POINT('Ctrl Pts',(26.7824404364531,63.9147221412979,210.009844426239));
#34636=CARTESIAN_POINT('Ctrl Pts',(26.787903481163,63.8383252279674,210.004820964463));
#34637=CARTESIAN_POINT('Ctrl Pts',(26.787903481163,63.7619809500992,210.));
#34638=CARTESIAN_POINT('Origin',(25.187903481163,63.761980950099,212.5));
#34639=CARTESIAN_POINT('',(26.787903481163,63.7619809500991,211.4));
#34640=CARTESIAN_POINT('',(26.787903481163,63.761980950099,211.312499998088));
#34641=CARTESIAN_POINT('',(26.787903481163,63.761980950099,212.5));
#34642=CARTESIAN_POINT('Ctrl Pts',(26.787903481163,63.7619809500984,210.612499998088));
#34643=CARTESIAN_POINT('Ctrl Pts',(26.7879034811631,63.9037107253896,210.621449905392));
#34644=CARTESIAN_POINT('Ctrl Pts',(26.7690814709595,64.0450567131394,210.631061796522));
#34645=CARTESIAN_POINT('Ctrl Pts',(26.676120457749,64.3864277595664,210.656007791673));
#34646=CARTESIAN_POINT('Ctrl Pts',(26.5806505336575,64.5774371296308,210.671550265654));
#34647=CARTESIAN_POINT('Ctrl Pts',(26.3258621156874,64.9049914141014,210.701523721729));
#34648=CARTESIAN_POINT('Ctrl Pts',(26.1713533227639,65.0403771596247,210.71570615131));
#34649=CARTESIAN_POINT('Ctrl Pts',(25.8124811708408,65.2502286765258,210.74204166948));
#34650=CARTESIAN_POINT('Ctrl Pts',(25.6098048312725,65.3198939590718,210.756736357976));
#34651=CARTESIAN_POINT('Ctrl Pts',(25.1922317328634,65.3755565745708,210.787184396402));
#34652=CARTESIAN_POINT('Ctrl Pts',(24.9817212059254,65.3623385461095,210.802534122324));
#34653=CARTESIAN_POINT('Ctrl Pts',(24.5833395517246,65.2572210268484,210.83158278461));
#34654=CARTESIAN_POINT('Ctrl Pts',(24.3987100063986,65.1685359919833,210.844118647828));
#34655=CARTESIAN_POINT('Ctrl Pts',(24.0648789193331,64.9212610365502,210.871904414043));
#34656=CARTESIAN_POINT('Ctrl Pts',(23.9211076293836,64.7621342296066,210.887194565245));
#34657=CARTESIAN_POINT('Ctrl Pts',(23.7070740647399,64.4021292053075,210.917731356412));
#34658=CARTESIAN_POINT('Ctrl Pts',(23.6368802079579,64.2058290103964,210.93268641045));
#34659=CARTESIAN_POINT('Ctrl Pts',(23.5750272679402,63.7974449517029,210.960729973735));
#34660=CARTESIAN_POINT('Ctrl Pts',(23.5839027566284,63.5893072917234,210.973258080246));
#34661=CARTESIAN_POINT('Ctrl Pts',(23.6816051332063,63.1822774641359,211.002523137679));
#34662=CARTESIAN_POINT('Ctrl Pts',(23.7716313957965,62.9879341047716,211.018077678543));
#34663=CARTESIAN_POINT('Ctrl Pts',(24.0174773001968,62.6521340551642,211.048245806462));
#34664=CARTESIAN_POINT('Ctrl Pts',(24.168483443106,62.5119870400657,211.062601198416));
#34665=CARTESIAN_POINT('Ctrl Pts',(24.5234622974082,62.2908155773961,211.089509601821));
#34666=CARTESIAN_POINT('Ctrl Pts',(24.7260650487856,62.2151797158321,211.103824279061));
#34667=CARTESIAN_POINT('Ctrl Pts',(25.1444797102404,62.1489193406298,211.134333681458));
#34668=CARTESIAN_POINT('Ctrl Pts',(25.3557546484568,62.1570865885378,211.149739145703));
#34669=CARTESIAN_POINT('Ctrl Pts',(25.7567847791617,62.2528316013046,211.178980926067));
#34670=CARTESIAN_POINT('Ctrl Pts',(25.9432793469075,62.3370116972185,211.191722899357));
#34671=CARTESIAN_POINT('Ctrl Pts',(26.2827471489827,62.5760539273622,211.219194293258));
#34672=CARTESIAN_POINT('Ctrl Pts',(26.4302825723362,62.7316607245787,211.234399398023));
#34673=CARTESIAN_POINT('Ctrl Pts',(26.6531563261176,63.0867932265012,211.26495079924));
#34674=CARTESIAN_POINT('Ctrl Pts',(26.7281414813671,63.2818387401592,211.280001305818));
#34675=CARTESIAN_POINT('Ctrl Pts',(26.7799044875922,63.5771945052862,211.300539531777));
#34676=CARTESIAN_POINT('Ctrl Pts',(26.787903481163,63.6695974072158,211.306666191159));
#34677=CARTESIAN_POINT('Ctrl Pts',(26.787903481163,63.761980950099,211.312499998088));
#34678=CARTESIAN_POINT('Ctrl Pts',(26.787903481163,63.7619809500992,211.4));
#34679=CARTESIAN_POINT('Ctrl Pts',(26.787903481163,63.5818177827691,211.388623112936));
#34680=CARTESIAN_POINT('Ctrl Pts',(26.7574834653626,63.4027735141896,211.376207818663));
#34681=CARTESIAN_POINT('Ctrl Pts',(26.6280540227834,63.0338003226158,211.348189233772));
#34682=CARTESIAN_POINT('Ctrl Pts',(26.5199058336431,62.8509089809943,211.332697166086));
#34683=CARTESIAN_POINT('Ctrl Pts',(26.2387935136483,62.5372102260688,211.302638929041));
#34684=CARTESIAN_POINT('Ctrl Pts',(26.0685425028871,62.409623601325,211.289213262001));
#34685=CARTESIAN_POINT('Ctrl Pts',(25.6934670952748,62.2301618676489,211.261864013529));
#34686=CARTESIAN_POINT('Ctrl Pts',(25.4931983745446,62.1780553272494,211.247261085976));
#34687=CARTESIAN_POINT('Ctrl Pts',(25.0759790833614,62.1517443047337,211.216838845994));
#34688=CARTESIAN_POINT('Ctrl Pts',(24.8627737506939,62.1809358106765,211.20129262382));
#34689=CARTESIAN_POINT('Ctrl Pts',(24.4682306869984,62.318384231228,211.172523858759));
#34690=CARTESIAN_POINT('Ctrl Pts',(24.2896915048165,62.4221615228617,211.160192517772));
#34691=CARTESIAN_POINT('Ctrl Pts',(23.9792294077263,62.6932657854073,211.131753980388));
#34692=CARTESIAN_POINT('Ctrl Pts',(23.850999101966,62.8588144578357,211.116624901623));
#34693=CARTESIAN_POINT('Ctrl Pts',(23.6627242118601,63.2338890512605,211.086075620385));
#34694=CARTESIAN_POINT('Ctrl Pts',(23.6061720701984,63.4406992708552,211.070954236808));
#34695=CARTESIAN_POINT('Ctrl Pts',(23.5777851557484,63.8548157504408,211.043768799926));
#34696=CARTESIAN_POINT('Ctrl Pts',(23.6024758470122,64.0578851219841,211.030783052187));
#34697=CARTESIAN_POINT('Ctrl Pts',(23.7286150058584,64.4508373542569,211.001370204632));
#34698=CARTESIAN_POINT('Ctrl Pts',(23.8314542072517,64.6361025043355,210.985921793281));
#34699=CARTESIAN_POINT('Ctrl Pts',(24.1045537716373,64.9584604062835,210.955608882856));
#34700=CARTESIAN_POINT('Ctrl Pts',(24.2728951014121,65.0916092228732,210.941719361024));
#34701=CARTESIAN_POINT('Ctrl Pts',(24.6446256883595,65.2807669139696,210.914614005725));
#34702=CARTESIAN_POINT('Ctrl Pts',(24.8430428829701,65.3377000506952,210.900146085285));
#34703=CARTESIAN_POINT('Ctrl Pts',(25.2584164857913,65.3744897977321,210.869858426746));
#34704=CARTESIAN_POINT('Ctrl Pts',(25.4717415535027,65.3508837642616,210.854303473892));
#34705=CARTESIAN_POINT('Ctrl Pts',(25.8701292242356,65.2237778267173,210.825254372901));
#34706=CARTESIAN_POINT('Ctrl Pts',(26.0520865945744,65.1241359209362,210.812843591287));
#34707=CARTESIAN_POINT('Ctrl Pts',(26.3694620049696,64.8605053532319,210.784624952554));
#34708=CARTESIAN_POINT('Ctrl Pts',(26.5014814935139,64.6986363516567,210.7695900892));
#34709=CARTESIAN_POINT('Ctrl Pts',(26.6990750005974,64.3289275833056,210.739039906152));
#34710=CARTESIAN_POINT('Ctrl Pts',(26.760906433387,64.123600783922,210.723819722973));
#34711=CARTESIAN_POINT('Ctrl Pts',(26.7855541995538,63.8621531395226,210.706411292825));
#34712=CARTESIAN_POINT('Ctrl Pts',(26.787903481163,63.8120419129629,210.703161233948));
#34713=CARTESIAN_POINT('Ctrl Pts',(26.787903481163,63.7619809500997,210.7));
#34714=CARTESIAN_POINT('Origin',(25.187903481163,63.761980950099,212.5));
#34715=CARTESIAN_POINT('',(26.787903481163,63.761980950099,212.1));
#34716=CARTESIAN_POINT('',(26.787903481163,63.7619809500991,212.012499998088));
#34717=CARTESIAN_POINT('',(26.787903481163,63.761980950099,212.5));
#34718=CARTESIAN_POINT('',(26.3295442486903,64.882987800176,212.1));
#34719=CARTESIAN_POINT('Origin',(25.187903481163,63.761980950099,212.1));
#34720=CARTESIAN_POINT('Ctrl Pts',(26.787903481163,63.7619809500991,212.012499998088));
#34721=CARTESIAN_POINT('Ctrl Pts',(26.787903481163,63.8455254713351,212.017775641257));
#34722=CARTESIAN_POINT('Ctrl Pts',(26.7813616254594,63.929111069376,212.023292383486));
#34723=CARTESIAN_POINT('Ctrl Pts',(26.7425017960021,64.174747183526,212.040220500233));
#34724=CARTESIAN_POINT('Ctrl Pts',(26.6917702440339,64.3325238033038,212.05203331646));
#34725=CARTESIAN_POINT('Ctrl Pts',(26.5433031849841,64.6283088414431,212.076124318609));
#34726=CARTESIAN_POINT('Ctrl Pts',(26.4460274836205,64.7643605056857,212.088262176286));
#34727=CARTESIAN_POINT('Ctrl Pts',(26.3295442486903,64.882987800176,212.1));
#34728=CARTESIAN_POINT('Origin',(25.1879034811629,63.761980950099,212.406249999044));
#34729=CARTESIAN_POINT('',(23.966789593663,63.761980950099,203.043749999044));
#34730=CARTESIAN_POINT('',(23.966789593663,63.761980950099,202.868749999044));
#34731=CARTESIAN_POINT('',(23.9667895936629,63.761980950099,212.406249999044));
#34732=CARTESIAN_POINT('',(26.409017368663,63.761980950099,202.518749999044));
#34733=CARTESIAN_POINT('Ctrl Pts',(23.966789593663,63.761980950099,202.868749999044));
#34734=CARTESIAN_POINT('Ctrl Pts',(23.966789593663,64.4669913817583,202.810416665711));
#34735=CARTESIAN_POINT('Ctrl Pts',(24.577346537413,64.819496597588,202.752083332377));
#34736=CARTESIAN_POINT('Ctrl Pts',(25.187903481163,65.1720018134176,202.693749999044));
#34737=CARTESIAN_POINT('Ctrl Pts',(25.798460424913,64.819496597588,202.635416665711));
#34738=CARTESIAN_POINT('Ctrl Pts',(26.409017368663,64.4669913817583,202.577083332377));
#34739=CARTESIAN_POINT('Ctrl Pts',(26.409017368663,63.761980950099,202.518749999044));
#34740=CARTESIAN_POINT('',(26.409017368663,63.761980950099,202.693749999044));
#34741=CARTESIAN_POINT('',(26.409017368663,63.761980950099,202.606249999044));
#34742=CARTESIAN_POINT('Ctrl Pts',(23.966789593663,63.761980950099,203.043749999044));
#34743=CARTESIAN_POINT('Ctrl Pts',(23.966789593663,64.4669913817583,202.985416665711));
#34744=CARTESIAN_POINT('Ctrl Pts',(24.577346537413,64.819496597588,202.927083332377));
#34745=CARTESIAN_POINT('Ctrl Pts',(25.187903481163,65.1720018134176,202.868749999044));
#34746=CARTESIAN_POINT('Ctrl Pts',(25.798460424913,64.819496597588,202.810416665711));
#34747=CARTESIAN_POINT('Ctrl Pts',(26.409017368663,64.4669913817583,202.752083332377));
#34748=CARTESIAN_POINT('Ctrl Pts',(26.409017368663,63.761980950099,202.693749999044));
#34749=CARTESIAN_POINT('Origin',(25.1879034811629,63.761980950099,212.406249999044));
#34750=CARTESIAN_POINT('',(23.966789593663,63.761980950099,203.743749999044));
#34751=CARTESIAN_POINT('',(23.966789593663,63.761980950099,203.568749999044));
#34752=CARTESIAN_POINT('',(23.9667895936629,63.761980950099,212.406249999044));
#34753=CARTESIAN_POINT('Ctrl Pts',(23.966789593663,63.761980950099,203.568749999044));
#34754=CARTESIAN_POINT('Ctrl Pts',(23.966789593663,64.4669913817583,203.510416665711));
#34755=CARTESIAN_POINT('Ctrl Pts',(24.577346537413,64.819496597588,203.452083332377));
#34756=CARTESIAN_POINT('Ctrl Pts',(25.187903481163,65.1720018134176,203.393749999044));
#34757=CARTESIAN_POINT('Ctrl Pts',(25.798460424913,64.819496597588,203.335416665711));
#34758=CARTESIAN_POINT('Ctrl Pts',(26.409017368663,64.4669913817583,203.277083332377));
#34759=CARTESIAN_POINT('Ctrl Pts',(26.409017368663,63.761980950099,203.218749999044));
#34760=CARTESIAN_POINT('Ctrl Pts',(26.409017368663,63.0569705184397,203.160416665711));
#34761=CARTESIAN_POINT('Ctrl Pts',(25.798460424913,62.70446530261,203.102083332377));
#34762=CARTESIAN_POINT('Ctrl Pts',(25.187903481163,62.3519600867804,203.043749999044));
#34763=CARTESIAN_POINT('Ctrl Pts',(24.577346537413,62.70446530261,202.985416665711));
#34764=CARTESIAN_POINT('Ctrl Pts',(23.966789593663,63.0569705184397,202.927083332377));
#34765=CARTESIAN_POINT('Ctrl Pts',(23.966789593663,63.761980950099,202.868749999044));
#34766=CARTESIAN_POINT('Ctrl Pts',(23.966789593663,63.761980950099,203.743749999044));
#34767=CARTESIAN_POINT('Ctrl Pts',(23.966789593663,64.4669913817583,203.685416665711));
#34768=CARTESIAN_POINT('Ctrl Pts',(24.577346537413,64.819496597588,203.627083332377));
#34769=CARTESIAN_POINT('Ctrl Pts',(25.187903481163,65.1720018134176,203.568749999044));
#34770=CARTESIAN_POINT('Ctrl Pts',(25.798460424913,64.819496597588,203.510416665711));
#34771=CARTESIAN_POINT('Ctrl Pts',(26.409017368663,64.4669913817583,203.452083332377));
#34772=CARTESIAN_POINT('Ctrl Pts',(26.409017368663,63.761980950099,203.393749999044));
#34773=CARTESIAN_POINT('Ctrl Pts',(26.409017368663,63.0569705184397,203.335416665711));
#34774=CARTESIAN_POINT('Ctrl Pts',(25.798460424913,62.70446530261,203.277083332377));
#34775=CARTESIAN_POINT('Ctrl Pts',(25.187903481163,62.3519600867804,203.218749999044));
#34776=CARTESIAN_POINT('Ctrl Pts',(24.577346537413,62.70446530261,203.160416665711));
#34777=CARTESIAN_POINT('Ctrl Pts',(23.966789593663,63.0569705184397,203.102083332377));
#34778=CARTESIAN_POINT('Ctrl Pts',(23.966789593663,63.761980950099,203.043749999044));
#34779=CARTESIAN_POINT('Origin',(25.1879034811629,63.761980950099,212.406249999044));
#34780=CARTESIAN_POINT('',(23.966789593663,63.761980950099,204.443749999044));
#34781=CARTESIAN_POINT('',(23.966789593663,63.761980950099,204.268749999044));
#34782=CARTESIAN_POINT('',(23.9667895936629,63.761980950099,212.406249999044));
#34783=CARTESIAN_POINT('Ctrl Pts',(23.966789593663,63.761980950099,204.268749999044));
#34784=CARTESIAN_POINT('Ctrl Pts',(23.966789593663,64.4669913817583,204.210416665711));
#34785=CARTESIAN_POINT('Ctrl Pts',(24.577346537413,64.819496597588,204.152083332377));
#34786=CARTESIAN_POINT('Ctrl Pts',(25.187903481163,65.1720018134176,204.093749999044));
#34787=CARTESIAN_POINT('Ctrl Pts',(25.798460424913,64.819496597588,204.035416665711));
#34788=CARTESIAN_POINT('Ctrl Pts',(26.409017368663,64.4669913817583,203.977083332377));
#34789=CARTESIAN_POINT('Ctrl Pts',(26.409017368663,63.761980950099,203.918749999044));
#34790=CARTESIAN_POINT('Ctrl Pts',(26.409017368663,63.0569705184397,203.860416665711));
#34791=CARTESIAN_POINT('Ctrl Pts',(25.798460424913,62.70446530261,203.802083332377));
#34792=CARTESIAN_POINT('Ctrl Pts',(25.187903481163,62.3519600867804,203.743749999044));
#34793=CARTESIAN_POINT('Ctrl Pts',(24.577346537413,62.70446530261,203.685416665711));
#34794=CARTESIAN_POINT('Ctrl Pts',(23.966789593663,63.0569705184397,203.627083332377));
#34795=CARTESIAN_POINT('Ctrl Pts',(23.966789593663,63.761980950099,203.568749999044));
#34796=CARTESIAN_POINT('Ctrl Pts',(23.966789593663,63.761980950099,204.443749999044));
#34797=CARTESIAN_POINT('Ctrl Pts',(23.966789593663,64.4669913817583,204.385416665711));
#34798=CARTESIAN_POINT('Ctrl Pts',(24.577346537413,64.819496597588,204.327083332377));
#34799=CARTESIAN_POINT('Ctrl Pts',(25.187903481163,65.1720018134176,204.268749999044));
#34800=CARTESIAN_POINT('Ctrl Pts',(25.798460424913,64.819496597588,204.210416665711));
#34801=CARTESIAN_POINT('Ctrl Pts',(26.409017368663,64.4669913817583,204.152083332377));
#34802=CARTESIAN_POINT('Ctrl Pts',(26.409017368663,63.761980950099,204.093749999044));
#34803=CARTESIAN_POINT('Ctrl Pts',(26.409017368663,63.0569705184397,204.035416665711));
#34804=CARTESIAN_POINT('Ctrl Pts',(25.798460424913,62.70446530261,203.977083332377));
#34805=CARTESIAN_POINT('Ctrl Pts',(25.187903481163,62.3519600867804,203.918749999044));
#34806=CARTESIAN_POINT('Ctrl Pts',(24.577346537413,62.70446530261,203.860416665711));
#34807=CARTESIAN_POINT('Ctrl Pts',(23.966789593663,63.0569705184397,203.802083332377));
#34808=CARTESIAN_POINT('Ctrl Pts',(23.966789593663,63.761980950099,203.743749999044));
#34809=CARTESIAN_POINT('Origin',(25.1879034811629,63.761980950099,212.406249999044));
#34810=CARTESIAN_POINT('',(23.966789593663,63.761980950099,205.143749999044));
#34811=CARTESIAN_POINT('',(23.966789593663,63.761980950099,204.968749999044));
#34812=CARTESIAN_POINT('',(23.9667895936629,63.761980950099,212.406249999044));
#34813=CARTESIAN_POINT('Ctrl Pts',(23.966789593663,63.761980950099,204.968749999044));
#34814=CARTESIAN_POINT('Ctrl Pts',(23.966789593663,64.4669913817583,204.910416665711));
#34815=CARTESIAN_POINT('Ctrl Pts',(24.577346537413,64.819496597588,204.852083332377));
#34816=CARTESIAN_POINT('Ctrl Pts',(25.187903481163,65.1720018134176,204.793749999044));
#34817=CARTESIAN_POINT('Ctrl Pts',(25.798460424913,64.819496597588,204.735416665711));
#34818=CARTESIAN_POINT('Ctrl Pts',(26.409017368663,64.4669913817583,204.677083332377));
#34819=CARTESIAN_POINT('Ctrl Pts',(26.409017368663,63.761980950099,204.618749999044));
#34820=CARTESIAN_POINT('Ctrl Pts',(26.409017368663,63.0569705184397,204.560416665711));
#34821=CARTESIAN_POINT('Ctrl Pts',(25.798460424913,62.70446530261,204.502083332377));
#34822=CARTESIAN_POINT('Ctrl Pts',(25.187903481163,62.3519600867804,204.443749999044));
#34823=CARTESIAN_POINT('Ctrl Pts',(24.577346537413,62.70446530261,204.385416665711));
#34824=CARTESIAN_POINT('Ctrl Pts',(23.966789593663,63.0569705184397,204.327083332377));
#34825=CARTESIAN_POINT('Ctrl Pts',(23.966789593663,63.761980950099,204.268749999044));
#34826=CARTESIAN_POINT('Ctrl Pts',(23.966789593663,63.761980950099,205.143749999044));
#34827=CARTESIAN_POINT('Ctrl Pts',(23.966789593663,64.4669913817583,205.085416665711));
#34828=CARTESIAN_POINT('Ctrl Pts',(24.577346537413,64.819496597588,205.027083332377));
#34829=CARTESIAN_POINT('Ctrl Pts',(25.187903481163,65.1720018134176,204.968749999044));
#34830=CARTESIAN_POINT('Ctrl Pts',(25.798460424913,64.819496597588,204.910416665711));
#34831=CARTESIAN_POINT('Ctrl Pts',(26.409017368663,64.4669913817583,204.852083332377));
#34832=CARTESIAN_POINT('Ctrl Pts',(26.409017368663,63.761980950099,204.793749999044));
#34833=CARTESIAN_POINT('Ctrl Pts',(26.409017368663,63.0569705184397,204.735416665711));
#34834=CARTESIAN_POINT('Ctrl Pts',(25.798460424913,62.70446530261,204.677083332377));
#34835=CARTESIAN_POINT('Ctrl Pts',(25.187903481163,62.3519600867804,204.618749999044));
#34836=CARTESIAN_POINT('Ctrl Pts',(24.577346537413,62.70446530261,204.560416665711));
#34837=CARTESIAN_POINT('Ctrl Pts',(23.966789593663,63.0569705184397,204.502083332377));
#34838=CARTESIAN_POINT('Ctrl Pts',(23.966789593663,63.761980950099,204.443749999044));
#34839=CARTESIAN_POINT('Origin',(25.1879034811629,63.761980950099,212.406249999044));
#34840=CARTESIAN_POINT('',(23.966789593663,63.761980950099,205.843749999044));
#34841=CARTESIAN_POINT('',(23.966789593663,63.761980950099,205.668749999044));
#34842=CARTESIAN_POINT('',(23.9667895936629,63.761980950099,212.406249999044));
#34843=CARTESIAN_POINT('Ctrl Pts',(23.966789593663,63.761980950099,205.668749999044));
#34844=CARTESIAN_POINT('Ctrl Pts',(23.966789593663,64.4669913817583,205.610416665711));
#34845=CARTESIAN_POINT('Ctrl Pts',(24.577346537413,64.819496597588,205.552083332377));
#34846=CARTESIAN_POINT('Ctrl Pts',(25.187903481163,65.1720018134176,205.493749999044));
#34847=CARTESIAN_POINT('Ctrl Pts',(25.798460424913,64.819496597588,205.435416665711));
#34848=CARTESIAN_POINT('Ctrl Pts',(26.409017368663,64.4669913817583,205.377083332377));
#34849=CARTESIAN_POINT('Ctrl Pts',(26.409017368663,63.761980950099,205.318749999044));
#34850=CARTESIAN_POINT('Ctrl Pts',(26.409017368663,63.0569705184397,205.260416665711));
#34851=CARTESIAN_POINT('Ctrl Pts',(25.798460424913,62.70446530261,205.202083332377));
#34852=CARTESIAN_POINT('Ctrl Pts',(25.187903481163,62.3519600867804,205.143749999044));
#34853=CARTESIAN_POINT('Ctrl Pts',(24.577346537413,62.70446530261,205.085416665711));
#34854=CARTESIAN_POINT('Ctrl Pts',(23.966789593663,63.0569705184397,205.027083332377));
#34855=CARTESIAN_POINT('Ctrl Pts',(23.966789593663,63.761980950099,204.968749999044));
#34856=CARTESIAN_POINT('Ctrl Pts',(23.966789593663,63.761980950099,205.843749999044));
#34857=CARTESIAN_POINT('Ctrl Pts',(23.966789593663,64.4669913817583,205.785416665711));
#34858=CARTESIAN_POINT('Ctrl Pts',(24.577346537413,64.819496597588,205.727083332377));
#34859=CARTESIAN_POINT('Ctrl Pts',(25.187903481163,65.1720018134176,205.668749999044));
#34860=CARTESIAN_POINT('Ctrl Pts',(25.798460424913,64.819496597588,205.610416665711));
#34861=CARTESIAN_POINT('Ctrl Pts',(26.409017368663,64.4669913817583,205.552083332377));
#34862=CARTESIAN_POINT('Ctrl Pts',(26.409017368663,63.761980950099,205.493749999044));
#34863=CARTESIAN_POINT('Ctrl Pts',(26.409017368663,63.0569705184397,205.435416665711));
#34864=CARTESIAN_POINT('Ctrl Pts',(25.798460424913,62.70446530261,205.377083332377));
#34865=CARTESIAN_POINT('Ctrl Pts',(25.187903481163,62.3519600867804,205.318749999044));
#34866=CARTESIAN_POINT('Ctrl Pts',(24.577346537413,62.70446530261,205.260416665711));
#34867=CARTESIAN_POINT('Ctrl Pts',(23.966789593663,63.0569705184397,205.202083332377));
#34868=CARTESIAN_POINT('Ctrl Pts',(23.966789593663,63.761980950099,205.143749999044));
#34869=CARTESIAN_POINT('Origin',(25.1879034811629,63.761980950099,212.406249999044));
#34870=CARTESIAN_POINT('',(23.966789593663,63.761980950099,206.543749999044));
#34871=CARTESIAN_POINT('',(23.966789593663,63.761980950099,206.368749999044));
#34872=CARTESIAN_POINT('',(23.9667895936629,63.761980950099,212.406249999044));
#34873=CARTESIAN_POINT('Ctrl Pts',(23.966789593663,63.761980950099,206.368749999044));
#34874=CARTESIAN_POINT('Ctrl Pts',(23.966789593663,64.4669913817583,206.310416665711));
#34875=CARTESIAN_POINT('Ctrl Pts',(24.577346537413,64.819496597588,206.252083332377));
#34876=CARTESIAN_POINT('Ctrl Pts',(25.187903481163,65.1720018134176,206.193749999044));
#34877=CARTESIAN_POINT('Ctrl Pts',(25.798460424913,64.819496597588,206.135416665711));
#34878=CARTESIAN_POINT('Ctrl Pts',(26.409017368663,64.4669913817583,206.077083332377));
#34879=CARTESIAN_POINT('Ctrl Pts',(26.409017368663,63.761980950099,206.018749999044));
#34880=CARTESIAN_POINT('Ctrl Pts',(26.409017368663,63.0569705184397,205.960416665711));
#34881=CARTESIAN_POINT('Ctrl Pts',(25.798460424913,62.70446530261,205.902083332377));
#34882=CARTESIAN_POINT('Ctrl Pts',(25.187903481163,62.3519600867804,205.843749999044));
#34883=CARTESIAN_POINT('Ctrl Pts',(24.577346537413,62.70446530261,205.785416665711));
#34884=CARTESIAN_POINT('Ctrl Pts',(23.966789593663,63.0569705184397,205.727083332377));
#34885=CARTESIAN_POINT('Ctrl Pts',(23.966789593663,63.761980950099,205.668749999044));
#34886=CARTESIAN_POINT('Ctrl Pts',(23.966789593663,63.761980950099,206.543749999044));
#34887=CARTESIAN_POINT('Ctrl Pts',(23.966789593663,64.4669913817583,206.485416665711));
#34888=CARTESIAN_POINT('Ctrl Pts',(24.577346537413,64.819496597588,206.427083332377));
#34889=CARTESIAN_POINT('Ctrl Pts',(25.187903481163,65.1720018134176,206.368749999044));
#34890=CARTESIAN_POINT('Ctrl Pts',(25.798460424913,64.819496597588,206.310416665711));
#34891=CARTESIAN_POINT('Ctrl Pts',(26.409017368663,64.4669913817583,206.252083332377));
#34892=CARTESIAN_POINT('Ctrl Pts',(26.409017368663,63.761980950099,206.193749999044));
#34893=CARTESIAN_POINT('Ctrl Pts',(26.409017368663,63.0569705184397,206.135416665711));
#34894=CARTESIAN_POINT('Ctrl Pts',(25.798460424913,62.70446530261,206.077083332377));
#34895=CARTESIAN_POINT('Ctrl Pts',(25.187903481163,62.3519600867804,206.018749999044));
#34896=CARTESIAN_POINT('Ctrl Pts',(24.577346537413,62.70446530261,205.960416665711));
#34897=CARTESIAN_POINT('Ctrl Pts',(23.966789593663,63.0569705184397,205.902083332377));
#34898=CARTESIAN_POINT('Ctrl Pts',(23.966789593663,63.761980950099,205.843749999044));
#34899=CARTESIAN_POINT('Origin',(25.1879034811629,63.761980950099,212.406249999044));
#34900=CARTESIAN_POINT('',(23.966789593663,63.761980950099,207.243749999044));
#34901=CARTESIAN_POINT('',(23.966789593663,63.761980950099,207.068749999044));
#34902=CARTESIAN_POINT('',(23.9667895936629,63.761980950099,212.406249999044));
#34903=CARTESIAN_POINT('Ctrl Pts',(23.966789593663,63.761980950099,207.068749999044));
#34904=CARTESIAN_POINT('Ctrl Pts',(23.966789593663,64.4669913817583,207.010416665711));
#34905=CARTESIAN_POINT('Ctrl Pts',(24.577346537413,64.819496597588,206.952083332377));
#34906=CARTESIAN_POINT('Ctrl Pts',(25.187903481163,65.1720018134176,206.893749999044));
#34907=CARTESIAN_POINT('Ctrl Pts',(25.798460424913,64.819496597588,206.835416665711));
#34908=CARTESIAN_POINT('Ctrl Pts',(26.409017368663,64.4669913817583,206.777083332377));
#34909=CARTESIAN_POINT('Ctrl Pts',(26.409017368663,63.761980950099,206.718749999044));
#34910=CARTESIAN_POINT('Ctrl Pts',(26.409017368663,63.0569705184397,206.660416665711));
#34911=CARTESIAN_POINT('Ctrl Pts',(25.798460424913,62.70446530261,206.602083332377));
#34912=CARTESIAN_POINT('Ctrl Pts',(25.187903481163,62.3519600867804,206.543749999044));
#34913=CARTESIAN_POINT('Ctrl Pts',(24.577346537413,62.70446530261,206.485416665711));
#34914=CARTESIAN_POINT('Ctrl Pts',(23.966789593663,63.0569705184397,206.427083332377));
#34915=CARTESIAN_POINT('Ctrl Pts',(23.966789593663,63.761980950099,206.368749999044));
#34916=CARTESIAN_POINT('Ctrl Pts',(23.966789593663,63.761980950099,207.243749999044));
#34917=CARTESIAN_POINT('Ctrl Pts',(23.966789593663,64.4669913817583,207.185416665711));
#34918=CARTESIAN_POINT('Ctrl Pts',(24.577346537413,64.819496597588,207.127083332377));
#34919=CARTESIAN_POINT('Ctrl Pts',(25.187903481163,65.1720018134176,207.068749999044));
#34920=CARTESIAN_POINT('Ctrl Pts',(25.798460424913,64.819496597588,207.010416665711));
#34921=CARTESIAN_POINT('Ctrl Pts',(26.409017368663,64.4669913817583,206.952083332377));
#34922=CARTESIAN_POINT('Ctrl Pts',(26.409017368663,63.761980950099,206.893749999044));
#34923=CARTESIAN_POINT('Ctrl Pts',(26.409017368663,63.0569705184397,206.835416665711));
#34924=CARTESIAN_POINT('Ctrl Pts',(25.798460424913,62.70446530261,206.777083332377));
#34925=CARTESIAN_POINT('Ctrl Pts',(25.187903481163,62.3519600867804,206.718749999044));
#34926=CARTESIAN_POINT('Ctrl Pts',(24.577346537413,62.70446530261,206.660416665711));
#34927=CARTESIAN_POINT('Ctrl Pts',(23.966789593663,63.0569705184397,206.602083332377));
#34928=CARTESIAN_POINT('Ctrl Pts',(23.966789593663,63.761980950099,206.543749999044));
#34929=CARTESIAN_POINT('Origin',(25.1879034811629,63.761980950099,212.406249999044));
#34930=CARTESIAN_POINT('',(23.966789593663,63.761980950099,207.943749999044));
#34931=CARTESIAN_POINT('',(23.966789593663,63.761980950099,207.768749999044));
#34932=CARTESIAN_POINT('',(23.9667895936629,63.761980950099,212.406249999044));
#34933=CARTESIAN_POINT('Ctrl Pts',(23.966789593663,63.761980950099,207.768749999044));
#34934=CARTESIAN_POINT('Ctrl Pts',(23.966789593663,64.4669913817583,207.710416665711));
#34935=CARTESIAN_POINT('Ctrl Pts',(24.577346537413,64.819496597588,207.652083332377));
#34936=CARTESIAN_POINT('Ctrl Pts',(25.187903481163,65.1720018134176,207.593749999044));
#34937=CARTESIAN_POINT('Ctrl Pts',(25.798460424913,64.819496597588,207.535416665711));
#34938=CARTESIAN_POINT('Ctrl Pts',(26.409017368663,64.4669913817583,207.477083332377));
#34939=CARTESIAN_POINT('Ctrl Pts',(26.409017368663,63.761980950099,207.418749999044));
#34940=CARTESIAN_POINT('Ctrl Pts',(26.409017368663,63.0569705184397,207.360416665711));
#34941=CARTESIAN_POINT('Ctrl Pts',(25.798460424913,62.70446530261,207.302083332377));
#34942=CARTESIAN_POINT('Ctrl Pts',(25.187903481163,62.3519600867804,207.243749999044));
#34943=CARTESIAN_POINT('Ctrl Pts',(24.577346537413,62.70446530261,207.185416665711));
#34944=CARTESIAN_POINT('Ctrl Pts',(23.966789593663,63.0569705184397,207.127083332377));
#34945=CARTESIAN_POINT('Ctrl Pts',(23.966789593663,63.761980950099,207.068749999044));
#34946=CARTESIAN_POINT('Ctrl Pts',(23.966789593663,63.761980950099,207.943749999044));
#34947=CARTESIAN_POINT('Ctrl Pts',(23.966789593663,64.4669913817583,207.885416665711));
#34948=CARTESIAN_POINT('Ctrl Pts',(24.577346537413,64.819496597588,207.827083332377));
#34949=CARTESIAN_POINT('Ctrl Pts',(25.187903481163,65.1720018134176,207.768749999044));
#34950=CARTESIAN_POINT('Ctrl Pts',(25.798460424913,64.819496597588,207.710416665711));
#34951=CARTESIAN_POINT('Ctrl Pts',(26.409017368663,64.4669913817583,207.652083332377));
#34952=CARTESIAN_POINT('Ctrl Pts',(26.409017368663,63.761980950099,207.593749999044));
#34953=CARTESIAN_POINT('Ctrl Pts',(26.409017368663,63.0569705184397,207.535416665711));
#34954=CARTESIAN_POINT('Ctrl Pts',(25.798460424913,62.70446530261,207.477083332377));
#34955=CARTESIAN_POINT('Ctrl Pts',(25.187903481163,62.3519600867804,207.418749999044));
#34956=CARTESIAN_POINT('Ctrl Pts',(24.577346537413,62.70446530261,207.360416665711));
#34957=CARTESIAN_POINT('Ctrl Pts',(23.966789593663,63.0569705184397,207.302083332377));
#34958=CARTESIAN_POINT('Ctrl Pts',(23.966789593663,63.761980950099,207.243749999044));
#34959=CARTESIAN_POINT('Origin',(25.1879034811629,63.761980950099,212.406249999044));
#34960=CARTESIAN_POINT('',(23.966789593663,63.761980950099,208.643749999044));
#34961=CARTESIAN_POINT('',(23.966789593663,63.761980950099,208.468749999044));
#34962=CARTESIAN_POINT('',(23.9667895936629,63.761980950099,212.406249999044));
#34963=CARTESIAN_POINT('Ctrl Pts',(23.966789593663,63.761980950099,208.468749999044));
#34964=CARTESIAN_POINT('Ctrl Pts',(23.966789593663,64.4669913817583,208.410416665711));
#34965=CARTESIAN_POINT('Ctrl Pts',(24.577346537413,64.819496597588,208.352083332377));
#34966=CARTESIAN_POINT('Ctrl Pts',(25.187903481163,65.1720018134176,208.293749999044));
#34967=CARTESIAN_POINT('Ctrl Pts',(25.798460424913,64.819496597588,208.235416665711));
#34968=CARTESIAN_POINT('Ctrl Pts',(26.409017368663,64.4669913817583,208.177083332377));
#34969=CARTESIAN_POINT('Ctrl Pts',(26.409017368663,63.761980950099,208.118749999044));
#34970=CARTESIAN_POINT('Ctrl Pts',(26.409017368663,63.0569705184397,208.060416665711));
#34971=CARTESIAN_POINT('Ctrl Pts',(25.798460424913,62.70446530261,208.002083332377));
#34972=CARTESIAN_POINT('Ctrl Pts',(25.187903481163,62.3519600867804,207.943749999044));
#34973=CARTESIAN_POINT('Ctrl Pts',(24.577346537413,62.70446530261,207.885416665711));
#34974=CARTESIAN_POINT('Ctrl Pts',(23.966789593663,63.0569705184397,207.827083332377));
#34975=CARTESIAN_POINT('Ctrl Pts',(23.966789593663,63.761980950099,207.768749999044));
#34976=CARTESIAN_POINT('Ctrl Pts',(23.966789593663,63.761980950099,208.643749999044));
#34977=CARTESIAN_POINT('Ctrl Pts',(23.966789593663,64.4669913817583,208.585416665711));
#34978=CARTESIAN_POINT('Ctrl Pts',(24.577346537413,64.819496597588,208.527083332377));
#34979=CARTESIAN_POINT('Ctrl Pts',(25.187903481163,65.1720018134176,208.468749999044));
#34980=CARTESIAN_POINT('Ctrl Pts',(25.798460424913,64.819496597588,208.410416665711));
#34981=CARTESIAN_POINT('Ctrl Pts',(26.409017368663,64.4669913817583,208.352083332377));
#34982=CARTESIAN_POINT('Ctrl Pts',(26.409017368663,63.761980950099,208.293749999044));
#34983=CARTESIAN_POINT('Ctrl Pts',(26.409017368663,63.0569705184397,208.235416665711));
#34984=CARTESIAN_POINT('Ctrl Pts',(25.798460424913,62.70446530261,208.177083332377));
#34985=CARTESIAN_POINT('Ctrl Pts',(25.187903481163,62.3519600867804,208.118749999044));
#34986=CARTESIAN_POINT('Ctrl Pts',(24.577346537413,62.70446530261,208.060416665711));
#34987=CARTESIAN_POINT('Ctrl Pts',(23.966789593663,63.0569705184397,208.002083332377));
#34988=CARTESIAN_POINT('Ctrl Pts',(23.966789593663,63.761980950099,207.943749999044));
#34989=CARTESIAN_POINT('Origin',(25.1879034811629,63.761980950099,212.406249999044));
#34990=CARTESIAN_POINT('',(23.966789593663,63.761980950099,209.343749999044));
#34991=CARTESIAN_POINT('',(23.966789593663,63.761980950099,209.168749999044));
#34992=CARTESIAN_POINT('',(23.9667895936629,63.761980950099,212.406249999044));
#34993=CARTESIAN_POINT('Ctrl Pts',(23.966789593663,63.761980950099,209.168749999044));
#34994=CARTESIAN_POINT('Ctrl Pts',(23.966789593663,64.4669913817583,209.110416665711));
#34995=CARTESIAN_POINT('Ctrl Pts',(24.577346537413,64.819496597588,209.052083332377));
#34996=CARTESIAN_POINT('Ctrl Pts',(25.187903481163,65.1720018134176,208.993749999044));
#34997=CARTESIAN_POINT('Ctrl Pts',(25.798460424913,64.819496597588,208.935416665711));
#34998=CARTESIAN_POINT('Ctrl Pts',(26.409017368663,64.4669913817583,208.877083332377));
#34999=CARTESIAN_POINT('Ctrl Pts',(26.409017368663,63.761980950099,208.818749999044));
#35000=CARTESIAN_POINT('Ctrl Pts',(26.409017368663,63.0569705184397,208.760416665711));
#35001=CARTESIAN_POINT('Ctrl Pts',(25.798460424913,62.70446530261,208.702083332377));
#35002=CARTESIAN_POINT('Ctrl Pts',(25.187903481163,62.3519600867804,208.643749999044));
#35003=CARTESIAN_POINT('Ctrl Pts',(24.577346537413,62.70446530261,208.585416665711));
#35004=CARTESIAN_POINT('Ctrl Pts',(23.966789593663,63.0569705184397,208.527083332377));
#35005=CARTESIAN_POINT('Ctrl Pts',(23.966789593663,63.761980950099,208.468749999044));
#35006=CARTESIAN_POINT('Ctrl Pts',(23.966789593663,63.761980950099,209.343749999044));
#35007=CARTESIAN_POINT('Ctrl Pts',(23.966789593663,64.4669913817583,209.285416665711));
#35008=CARTESIAN_POINT('Ctrl Pts',(24.577346537413,64.819496597588,209.227083332377));
#35009=CARTESIAN_POINT('Ctrl Pts',(25.187903481163,65.1720018134176,209.168749999044));
#35010=CARTESIAN_POINT('Ctrl Pts',(25.798460424913,64.819496597588,209.110416665711));
#35011=CARTESIAN_POINT('Ctrl Pts',(26.409017368663,64.4669913817583,209.052083332377));
#35012=CARTESIAN_POINT('Ctrl Pts',(26.409017368663,63.761980950099,208.993749999044));
#35013=CARTESIAN_POINT('Ctrl Pts',(26.409017368663,63.0569705184397,208.935416665711));
#35014=CARTESIAN_POINT('Ctrl Pts',(25.798460424913,62.70446530261,208.877083332377));
#35015=CARTESIAN_POINT('Ctrl Pts',(25.187903481163,62.3519600867804,208.818749999044));
#35016=CARTESIAN_POINT('Ctrl Pts',(24.577346537413,62.70446530261,208.760416665711));
#35017=CARTESIAN_POINT('Ctrl Pts',(23.966789593663,63.0569705184397,208.702083332377));
#35018=CARTESIAN_POINT('Ctrl Pts',(23.966789593663,63.761980950099,208.643749999044));
#35019=CARTESIAN_POINT('Origin',(25.1879034811629,63.761980950099,212.406249999044));
#35020=CARTESIAN_POINT('',(23.966789593663,63.761980950099,210.043749999044));
#35021=CARTESIAN_POINT('',(23.966789593663,63.761980950099,209.868749999044));
#35022=CARTESIAN_POINT('',(23.9667895936629,63.761980950099,212.406249999044));
#35023=CARTESIAN_POINT('Ctrl Pts',(23.966789593663,63.761980950099,209.868749999044));
#35024=CARTESIAN_POINT('Ctrl Pts',(23.966789593663,64.4669913817583,209.810416665711));
#35025=CARTESIAN_POINT('Ctrl Pts',(24.577346537413,64.819496597588,209.752083332377));
#35026=CARTESIAN_POINT('Ctrl Pts',(25.187903481163,65.1720018134176,209.693749999044));
#35027=CARTESIAN_POINT('Ctrl Pts',(25.798460424913,64.819496597588,209.635416665711));
#35028=CARTESIAN_POINT('Ctrl Pts',(26.409017368663,64.4669913817583,209.577083332377));
#35029=CARTESIAN_POINT('Ctrl Pts',(26.409017368663,63.761980950099,209.518749999044));
#35030=CARTESIAN_POINT('Ctrl Pts',(26.409017368663,63.0569705184397,209.460416665711));
#35031=CARTESIAN_POINT('Ctrl Pts',(25.798460424913,62.70446530261,209.402083332377));
#35032=CARTESIAN_POINT('Ctrl Pts',(25.187903481163,62.3519600867804,209.343749999044));
#35033=CARTESIAN_POINT('Ctrl Pts',(24.577346537413,62.70446530261,209.285416665711));
#35034=CARTESIAN_POINT('Ctrl Pts',(23.966789593663,63.0569705184397,209.227083332377));
#35035=CARTESIAN_POINT('Ctrl Pts',(23.966789593663,63.761980950099,209.168749999044));
#35036=CARTESIAN_POINT('Ctrl Pts',(23.966789593663,63.761980950099,210.043749999044));
#35037=CARTESIAN_POINT('Ctrl Pts',(23.966789593663,64.4669913817583,209.985416665711));
#35038=CARTESIAN_POINT('Ctrl Pts',(24.577346537413,64.819496597588,209.927083332377));
#35039=CARTESIAN_POINT('Ctrl Pts',(25.187903481163,65.1720018134176,209.868749999044));
#35040=CARTESIAN_POINT('Ctrl Pts',(25.798460424913,64.819496597588,209.810416665711));
#35041=CARTESIAN_POINT('Ctrl Pts',(26.409017368663,64.4669913817583,209.752083332377));
#35042=CARTESIAN_POINT('Ctrl Pts',(26.409017368663,63.761980950099,209.693749999044));
#35043=CARTESIAN_POINT('Ctrl Pts',(26.409017368663,63.0569705184397,209.635416665711));
#35044=CARTESIAN_POINT('Ctrl Pts',(25.798460424913,62.70446530261,209.577083332377));
#35045=CARTESIAN_POINT('Ctrl Pts',(25.187903481163,62.3519600867804,209.518749999044));
#35046=CARTESIAN_POINT('Ctrl Pts',(24.577346537413,62.70446530261,209.460416665711));
#35047=CARTESIAN_POINT('Ctrl Pts',(23.966789593663,63.0569705184397,209.402083332377));
#35048=CARTESIAN_POINT('Ctrl Pts',(23.966789593663,63.761980950099,209.343749999044));
#35049=CARTESIAN_POINT('Origin',(25.1879034811629,63.761980950099,212.406249999044));
#35050=CARTESIAN_POINT('',(23.966789593663,63.761980950099,210.743749999044));
#35051=CARTESIAN_POINT('',(23.966789593663,63.761980950099,210.568749999044));
#35052=CARTESIAN_POINT('',(23.9667895936629,63.761980950099,212.406249999044));
#35053=CARTESIAN_POINT('Ctrl Pts',(23.966789593663,63.761980950099,210.568749999044));
#35054=CARTESIAN_POINT('Ctrl Pts',(23.966789593663,64.4669913817583,210.510416665711));
#35055=CARTESIAN_POINT('Ctrl Pts',(24.577346537413,64.819496597588,210.452083332377));
#35056=CARTESIAN_POINT('Ctrl Pts',(25.187903481163,65.1720018134176,210.393749999044));
#35057=CARTESIAN_POINT('Ctrl Pts',(25.798460424913,64.819496597588,210.335416665711));
#35058=CARTESIAN_POINT('Ctrl Pts',(26.409017368663,64.4669913817583,210.277083332377));
#35059=CARTESIAN_POINT('Ctrl Pts',(26.409017368663,63.761980950099,210.218749999044));
#35060=CARTESIAN_POINT('Ctrl Pts',(26.409017368663,63.0569705184397,210.160416665711));
#35061=CARTESIAN_POINT('Ctrl Pts',(25.798460424913,62.70446530261,210.102083332377));
#35062=CARTESIAN_POINT('Ctrl Pts',(25.187903481163,62.3519600867804,210.043749999044));
#35063=CARTESIAN_POINT('Ctrl Pts',(24.577346537413,62.70446530261,209.985416665711));
#35064=CARTESIAN_POINT('Ctrl Pts',(23.966789593663,63.0569705184397,209.927083332377));
#35065=CARTESIAN_POINT('Ctrl Pts',(23.966789593663,63.761980950099,209.868749999044));
#35066=CARTESIAN_POINT('Ctrl Pts',(23.966789593663,63.761980950099,210.743749999044));
#35067=CARTESIAN_POINT('Ctrl Pts',(23.966789593663,64.4669913817583,210.685416665711));
#35068=CARTESIAN_POINT('Ctrl Pts',(24.577346537413,64.819496597588,210.627083332377));
#35069=CARTESIAN_POINT('Ctrl Pts',(25.187903481163,65.1720018134176,210.568749999044));
#35070=CARTESIAN_POINT('Ctrl Pts',(25.798460424913,64.819496597588,210.510416665711));
#35071=CARTESIAN_POINT('Ctrl Pts',(26.409017368663,64.4669913817583,210.452083332377));
#35072=CARTESIAN_POINT('Ctrl Pts',(26.409017368663,63.761980950099,210.393749999044));
#35073=CARTESIAN_POINT('Ctrl Pts',(26.409017368663,63.0569705184397,210.335416665711));
#35074=CARTESIAN_POINT('Ctrl Pts',(25.798460424913,62.70446530261,210.277083332377));
#35075=CARTESIAN_POINT('Ctrl Pts',(25.187903481163,62.3519600867804,210.218749999044));
#35076=CARTESIAN_POINT('Ctrl Pts',(24.577346537413,62.70446530261,210.160416665711));
#35077=CARTESIAN_POINT('Ctrl Pts',(23.966789593663,63.0569705184397,210.102083332377));
#35078=CARTESIAN_POINT('Ctrl Pts',(23.966789593663,63.761980950099,210.043749999044));
#35079=CARTESIAN_POINT('Origin',(25.1879034811629,63.761980950099,212.406249999044));
#35080=CARTESIAN_POINT('',(23.966789593663,63.761980950099,211.443749999044));
#35081=CARTESIAN_POINT('',(23.966789593663,63.761980950099,211.268749999044));
#35082=CARTESIAN_POINT('',(23.9667895936629,63.761980950099,212.406249999044));
#35083=CARTESIAN_POINT('Ctrl Pts',(23.966789593663,63.761980950099,211.268749999044));
#35084=CARTESIAN_POINT('Ctrl Pts',(23.966789593663,64.4669913817583,211.210416665711));
#35085=CARTESIAN_POINT('Ctrl Pts',(24.577346537413,64.819496597588,211.152083332377));
#35086=CARTESIAN_POINT('Ctrl Pts',(25.187903481163,65.1720018134176,211.093749999044));
#35087=CARTESIAN_POINT('Ctrl Pts',(25.798460424913,64.819496597588,211.035416665711));
#35088=CARTESIAN_POINT('Ctrl Pts',(26.409017368663,64.4669913817583,210.977083332377));
#35089=CARTESIAN_POINT('Ctrl Pts',(26.409017368663,63.761980950099,210.918749999044));
#35090=CARTESIAN_POINT('Ctrl Pts',(26.409017368663,63.0569705184397,210.860416665711));
#35091=CARTESIAN_POINT('Ctrl Pts',(25.798460424913,62.70446530261,210.802083332377));
#35092=CARTESIAN_POINT('Ctrl Pts',(25.187903481163,62.3519600867804,210.743749999044));
#35093=CARTESIAN_POINT('Ctrl Pts',(24.577346537413,62.70446530261,210.685416665711));
#35094=CARTESIAN_POINT('Ctrl Pts',(23.966789593663,63.0569705184397,210.627083332377));
#35095=CARTESIAN_POINT('Ctrl Pts',(23.966789593663,63.761980950099,210.568749999044));
#35096=CARTESIAN_POINT('Ctrl Pts',(23.966789593663,63.761980950099,211.443749999044));
#35097=CARTESIAN_POINT('Ctrl Pts',(23.966789593663,64.4669913817583,211.385416665711));
#35098=CARTESIAN_POINT('Ctrl Pts',(24.577346537413,64.819496597588,211.327083332377));
#35099=CARTESIAN_POINT('Ctrl Pts',(25.187903481163,65.1720018134176,211.268749999044));
#35100=CARTESIAN_POINT('Ctrl Pts',(25.798460424913,64.819496597588,211.210416665711));
#35101=CARTESIAN_POINT('Ctrl Pts',(26.409017368663,64.4669913817583,211.152083332377));
#35102=CARTESIAN_POINT('Ctrl Pts',(26.409017368663,63.761980950099,211.093749999044));
#35103=CARTESIAN_POINT('Ctrl Pts',(26.409017368663,63.0569705184397,211.035416665711));
#35104=CARTESIAN_POINT('Ctrl Pts',(25.798460424913,62.70446530261,210.977083332377));
#35105=CARTESIAN_POINT('Ctrl Pts',(25.187903481163,62.3519600867804,210.918749999044));
#35106=CARTESIAN_POINT('Ctrl Pts',(24.577346537413,62.70446530261,210.860416665711));
#35107=CARTESIAN_POINT('Ctrl Pts',(23.966789593663,63.0569705184397,210.802083332377));
#35108=CARTESIAN_POINT('Ctrl Pts',(23.966789593663,63.761980950099,210.743749999044));
#35109=CARTESIAN_POINT('Origin',(25.1879034811629,63.761980950099,212.406249999044));
#35110=CARTESIAN_POINT('',(23.966789593663,63.761980950099,212.143749999044));
#35111=CARTESIAN_POINT('',(23.966789593663,63.761980950099,211.968749999044));
#35112=CARTESIAN_POINT('',(23.9667895936629,63.761980950099,212.406249999044));
#35113=CARTESIAN_POINT('',(26.409017368663,63.761980950099,212.493749999044));
#35114=CARTESIAN_POINT('Ctrl Pts',(26.409017368663,63.761980950099,212.493749999044));
#35115=CARTESIAN_POINT('Ctrl Pts',(26.409017368663,63.0569705184397,212.435416665711));
#35116=CARTESIAN_POINT('Ctrl Pts',(25.798460424913,62.70446530261,212.377083332377));
#35117=CARTESIAN_POINT('Ctrl Pts',(25.187903481163,62.3519600867804,212.318749999044));
#35118=CARTESIAN_POINT('Ctrl Pts',(24.577346537413,62.70446530261,212.260416665711));
#35119=CARTESIAN_POINT('Ctrl Pts',(23.966789593663,63.0569705184397,212.202083332377));
#35120=CARTESIAN_POINT('Ctrl Pts',(23.966789593663,63.761980950099,212.143749999044));
#35121=CARTESIAN_POINT('',(26.409017368663,63.761980950099,212.318749999044));
#35122=CARTESIAN_POINT('',(26.409017368663,63.761980950099,212.406249999044));
#35123=CARTESIAN_POINT('Ctrl Pts',(26.409017368663,63.761980950099,212.318749999044));
#35124=CARTESIAN_POINT('Ctrl Pts',(26.409017368663,63.0569705184397,212.260416665711));
#35125=CARTESIAN_POINT('Ctrl Pts',(25.798460424913,62.70446530261,212.202083332377));
#35126=CARTESIAN_POINT('Ctrl Pts',(25.187903481163,62.3519600867804,212.143749999044));
#35127=CARTESIAN_POINT('Ctrl Pts',(24.577346537413,62.70446530261,212.085416665711));
#35128=CARTESIAN_POINT('Ctrl Pts',(23.966789593663,63.0569705184397,212.027083332377));
#35129=CARTESIAN_POINT('Ctrl Pts',(23.966789593663,63.761980950099,211.968749999044));
#35130=CARTESIAN_POINT('Origin',(43.0811453810944,77.1117683798101,211.));
#35131=CARTESIAN_POINT('',(41.4811453810944,77.1117683798101,212.));
#35132=CARTESIAN_POINT('Origin',(43.0811453810944,77.1117683798101,212.));
#35133=CARTESIAN_POINT('',(41.4811453810944,77.1117683798101,211.8));
#35134=CARTESIAN_POINT('',(41.4811453810944,77.1117683798101,211.));
#35135=CARTESIAN_POINT('Origin',(43.0811453810944,77.1117683798101,211.8));
#35136=CARTESIAN_POINT('Origin',(19.9513700273636,43.5818784659284,205.8));
#35137=CARTESIAN_POINT('',(18.4596441794768,43.5818784659284,212.8));
#35138=CARTESIAN_POINT('Origin',(19.9513700273636,43.5818784659284,212.8));
#35139=CARTESIAN_POINT('',(18.4596441794768,43.5818784659284,205.8));
#35140=CARTESIAN_POINT('',(18.4596441794768,43.5818784659284,205.8));
#35141=CARTESIAN_POINT('Origin',(19.9513700273636,43.5818784659284,205.8));
#35142=CARTESIAN_POINT('Origin',(43.0811453810902,77.1117683798122,214.746949994782));
#35143=CARTESIAN_POINT('',(44.1230495436541,77.1117683798122,210.3));
#35144=CARTESIAN_POINT('Origin',(43.0811453810904,77.1117683798123,210.3));
#35145=CARTESIAN_POINT('',(44.1230495436541,77.1117683798122,211.));
#35146=CARTESIAN_POINT('',(44.1230495436541,77.1117683798122,214.746949994782));
#35147=CARTESIAN_POINT('Origin',(43.0811453810902,77.1117683798122,211.));
#35148=CARTESIAN_POINT('Origin',(25.187903481163,63.761980950099,202.));
#35149=CARTESIAN_POINT('',(13.387903481163,63.761980950099,202.2));
#35150=CARTESIAN_POINT('Origin',(25.187903481163,63.761980950099,202.2));
#35151=CARTESIAN_POINT('',(13.187903481163,63.761980950099,202.));
#35152=CARTESIAN_POINT('Origin',(13.387903481163,63.761980950099,202.));
#35153=CARTESIAN_POINT('',(37.187903481163,63.761980950099,202.));
#35154=CARTESIAN_POINT('Origin',(25.187903481163,63.761980950099,202.));
#35155=CARTESIAN_POINT('Origin',(25.187903481163,63.761980950099,202.));
#35156=CARTESIAN_POINT('Origin',(25.187903481163,63.761980950099,201.4));
#35157=CARTESIAN_POINT('',(37.187903481163,63.761980950099,201.4));
#35158=CARTESIAN_POINT('',(13.187903481163,63.761980950099,201.4));
#35159=CARTESIAN_POINT('Origin',(25.187903481163,63.761980950099,201.4));
#35160=CARTESIAN_POINT('Origin',(25.187903481163,63.761980950099,201.4));
#35161=CARTESIAN_POINT('',(13.387903481163,63.761980950099,201.2));
#35162=CARTESIAN_POINT('Origin',(13.387903481163,63.761980950099,201.4));
#35163=CARTESIAN_POINT('Origin',(25.187903481163,63.761980950099,201.2));
#35164=CARTESIAN_POINT('Origin',(25.187903481163,63.761980950099,202.));
#35165=CARTESIAN_POINT('',(28.437903481163,63.761980950099,202.));
#35166=CARTESIAN_POINT('',(21.937903481163,63.761980950099,202.));
#35167=CARTESIAN_POINT('Origin',(25.187903481163,63.761980950099,202.));
#35168=CARTESIAN_POINT('Origin',(25.187903481163,63.761980950099,202.));
#35169=CARTESIAN_POINT('',(21.737903481163,63.761980950099,202.2));
#35170=CARTESIAN_POINT('Origin',(21.737903481163,63.761980950099,202.));
#35171=CARTESIAN_POINT('Origin',(25.187903481163,63.761980950099,202.2));
#35172=CARTESIAN_POINT('Origin',(25.187903481163,63.761980950099,201.4));
#35173=CARTESIAN_POINT('',(21.737903481163,63.761980950099,201.2));
#35174=CARTESIAN_POINT('Origin',(25.187903481163,63.761980950099,201.2));
#35175=CARTESIAN_POINT('',(21.937903481163,63.761980950099,201.4));
#35176=CARTESIAN_POINT('Origin',(21.737903481163,63.761980950099,201.4));
#35177=CARTESIAN_POINT('',(28.437903481163,63.761980950099,201.4));
#35178=CARTESIAN_POINT('Origin',(25.187903481163,63.761980950099,201.4));
#35179=CARTESIAN_POINT('Origin',(25.187903481163,63.761980950099,201.4));
#35180=CARTESIAN_POINT('Origin',(25.187903481163,63.761980950099,202.2));
#35181=CARTESIAN_POINT('',(28.437903481163,63.761980950099,202.2));
#35182=CARTESIAN_POINT('Origin',(25.187903481163,63.761980950099,202.2));
#35183=CARTESIAN_POINT('',(37.187903481163,63.761980950099,202.2));
#35184=CARTESIAN_POINT('Origin',(25.187903481163,63.761980950099,201.2));
#35185=CARTESIAN_POINT('Origin',(25.187903481163,63.761980950099,202.2));
#35186=CARTESIAN_POINT('',(18.2509458845758,64.6993278993105,202.2));
#35187=CARTESIAN_POINT('Origin',(25.18790348116,63.761980950101,202.2));
#35188=CARTESIAN_POINT('Origin',(25.187903481163,63.761980950099,202.2));
#35189=CARTESIAN_POINT('',(27.187903481163,63.761980950099,202.2));
#35190=CARTESIAN_POINT('Origin',(25.187903481163,63.761980950099,202.2));
#35191=CARTESIAN_POINT('Origin',(25.1879034811632,63.761980950099,212.406249999044));
#35192=CARTESIAN_POINT('',(26.787903481163,63.761980950099,212.712499998088));
#35193=CARTESIAN_POINT('Ctrl Pts',(26.787903481163,63.761980950099,212.712499998088));
#35194=CARTESIAN_POINT('Ctrl Pts',(26.787903481163,62.8382205193956,212.654166664755));
#35195=CARTESIAN_POINT('Ctrl Pts',(25.987903481163,62.3763403040439,212.595833331421));
#35196=CARTESIAN_POINT('Ctrl Pts',(25.187903481163,61.9144600886922,212.537499998088));
#35197=CARTESIAN_POINT('Ctrl Pts',(24.387903481163,62.3763403040439,212.479166664755));
#35198=CARTESIAN_POINT('Ctrl Pts',(23.587903481163,62.8382205193956,212.420833331421));
#35199=CARTESIAN_POINT('Ctrl Pts',(23.587903481163,63.761980950099,212.362499998088));
#35200=CARTESIAN_POINT('Ctrl Pts',(23.587903481163,64.6857413808024,212.304166664755));
#35201=CARTESIAN_POINT('Ctrl Pts',(24.387903481163,65.1476215961541,212.245833331421));
#35202=CARTESIAN_POINT('Ctrl Pts',(25.187903481163,65.6095018115058,212.187499998088));
#35203=CARTESIAN_POINT('Ctrl Pts',(25.987903481163,65.1476215961541,212.129166664755));
#35204=CARTESIAN_POINT('Ctrl Pts',(26.1767578512194,65.0385864747644,212.115396033605));
#35205=CARTESIAN_POINT('Ctrl Pts',(26.3295442486903,64.882987800176,212.1));
#35206=CARTESIAN_POINT('',(23.587903481163,63.761980950099,212.1));
#35207=CARTESIAN_POINT('Origin',(25.187903481163,63.761980950099,212.1));
#35208=CARTESIAN_POINT('Origin',(25.187903481163,63.761980950099,212.1));
#35209=CARTESIAN_POINT('',(26.787903481163,63.761980950099,212.406249999044));
#35210=CARTESIAN_POINT('Ctrl Pts',(26.787903481163,63.761980950099,212.712499998088));
#35211=CARTESIAN_POINT('Ctrl Pts',(26.787903481163,62.8382205193956,212.654166664755));
#35212=CARTESIAN_POINT('Ctrl Pts',(25.987903481163,62.3763403040439,212.595833331421));
#35213=CARTESIAN_POINT('Ctrl Pts',(25.187903481163,61.9144600886922,212.537499998088));
#35214=CARTESIAN_POINT('Ctrl Pts',(24.387903481163,62.3763403040439,212.479166664755));
#35215=CARTESIAN_POINT('Ctrl Pts',(23.587903481163,62.8382205193956,212.420833331421));
#35216=CARTESIAN_POINT('Ctrl Pts',(23.587903481163,63.761980950099,212.362499998088));
#35217=CARTESIAN_POINT('Ctrl Pts',(23.587903481163,64.6857413808024,212.304166664755));
#35218=CARTESIAN_POINT('Ctrl Pts',(24.387903481163,65.1476215961541,212.245833331421));
#35219=CARTESIAN_POINT('Ctrl Pts',(25.187903481163,65.6095018115058,212.187499998088));
#35220=CARTESIAN_POINT('Ctrl Pts',(25.987903481163,65.1476215961541,212.129166664755));
#35221=CARTESIAN_POINT('Ctrl Pts',(26.787903481163,64.6857413808024,212.070833331422));
#35222=CARTESIAN_POINT('Ctrl Pts',(26.787903481163,63.761980950099,212.012499998088));
#35223=CARTESIAN_POINT('Ctrl Pts',(26.787903481163,62.8382205193956,211.954166664755));
#35224=CARTESIAN_POINT('Ctrl Pts',(25.987903481163,62.3763403040439,211.895833331421));
#35225=CARTESIAN_POINT('Ctrl Pts',(25.187903481163,61.9144600886922,211.837499998088));
#35226=CARTESIAN_POINT('Ctrl Pts',(24.387903481163,62.3763403040439,211.779166664755));
#35227=CARTESIAN_POINT('Ctrl Pts',(23.587903481163,62.8382205193956,211.720833331422));
#35228=CARTESIAN_POINT('Ctrl Pts',(23.587903481163,63.761980950099,211.662499998088));
#35229=CARTESIAN_POINT('Ctrl Pts',(23.587903481163,64.6857413808024,211.604166664755));
#35230=CARTESIAN_POINT('Ctrl Pts',(24.387903481163,65.1476215961541,211.545833331421));
#35231=CARTESIAN_POINT('Ctrl Pts',(25.187903481163,65.6095018115058,211.487499998088));
#35232=CARTESIAN_POINT('Ctrl Pts',(25.987903481163,65.1476215961541,211.429166664755));
#35233=CARTESIAN_POINT('Ctrl Pts',(26.787903481163,64.6857413808024,211.370833331422));
#35234=CARTESIAN_POINT('Ctrl Pts',(26.787903481163,63.761980950099,211.312499998088));
#35235=CARTESIAN_POINT('Ctrl Pts',(26.787903481163,62.8382205193956,211.254166664755));
#35236=CARTESIAN_POINT('Ctrl Pts',(25.987903481163,62.3763403040439,211.195833331421));
#35237=CARTESIAN_POINT('Ctrl Pts',(25.187903481163,61.9144600886922,211.137499998088));
#35238=CARTESIAN_POINT('Ctrl Pts',(24.387903481163,62.3763403040439,211.079166664755));
#35239=CARTESIAN_POINT('Ctrl Pts',(23.587903481163,62.8382205193956,211.020833331422));
#35240=CARTESIAN_POINT('Ctrl Pts',(23.587903481163,63.761980950099,210.962499998088));
#35241=CARTESIAN_POINT('Ctrl Pts',(23.587903481163,64.6857413808024,210.904166664755));
#35242=CARTESIAN_POINT('Ctrl Pts',(24.387903481163,65.1476215961541,210.845833331421));
#35243=CARTESIAN_POINT('Ctrl Pts',(25.187903481163,65.6095018115058,210.787499998088));
#35244=CARTESIAN_POINT('Ctrl Pts',(25.987903481163,65.1476215961541,210.729166664755));
#35245=CARTESIAN_POINT('Ctrl Pts',(26.787903481163,64.6857413808024,210.670833331422));
#35246=CARTESIAN_POINT('Ctrl Pts',(26.787903481163,63.761980950099,210.612499998088));
#35247=CARTESIAN_POINT('Ctrl Pts',(26.787903481163,62.8382205193956,210.554166664755));
#35248=CARTESIAN_POINT('Ctrl Pts',(25.987903481163,62.3763403040439,210.495833331421));
#35249=CARTESIAN_POINT('Ctrl Pts',(25.187903481163,61.9144600886922,210.437499998088));
#35250=CARTESIAN_POINT('Ctrl Pts',(24.387903481163,62.3763403040439,210.379166664755));
#35251=CARTESIAN_POINT('Ctrl Pts',(23.587903481163,62.8382205193956,210.320833331422));
#35252=CARTESIAN_POINT('Ctrl Pts',(23.587903481163,63.761980950099,210.262499998088));
#35253=CARTESIAN_POINT('Ctrl Pts',(23.587903481163,64.6857413808024,210.204166664755));
#35254=CARTESIAN_POINT('Ctrl Pts',(24.387903481163,65.1476215961541,210.145833331421));
#35255=CARTESIAN_POINT('Ctrl Pts',(25.187903481163,65.6095018115058,210.087499998088));
#35256=CARTESIAN_POINT('Ctrl Pts',(25.987903481163,65.1476215961541,210.029166664755));
#35257=CARTESIAN_POINT('Ctrl Pts',(26.787903481163,64.6857413808024,209.970833331421));
#35258=CARTESIAN_POINT('Ctrl Pts',(26.787903481163,63.761980950099,209.912499998088));
#35259=CARTESIAN_POINT('Ctrl Pts',(26.787903481163,62.8382205193956,209.854166664755));
#35260=CARTESIAN_POINT('Ctrl Pts',(25.987903481163,62.3763403040439,209.795833331421));
#35261=CARTESIAN_POINT('Ctrl Pts',(25.187903481163,61.9144600886922,209.737499998088));
#35262=CARTESIAN_POINT('Ctrl Pts',(24.387903481163,62.3763403040439,209.679166664755));
#35263=CARTESIAN_POINT('Ctrl Pts',(23.587903481163,62.8382205193956,209.620833331422));
#35264=CARTESIAN_POINT('Ctrl Pts',(23.587903481163,63.761980950099,209.562499998088));
#35265=CARTESIAN_POINT('Ctrl Pts',(23.587903481163,64.6857413808024,209.504166664755));
#35266=CARTESIAN_POINT('Ctrl Pts',(24.387903481163,65.1476215961541,209.445833331422));
#35267=CARTESIAN_POINT('Ctrl Pts',(25.187903481163,65.6095018115058,209.387499998088));
#35268=CARTESIAN_POINT('Ctrl Pts',(25.987903481163,65.1476215961541,209.329166664755));
#35269=CARTESIAN_POINT('Ctrl Pts',(26.787903481163,64.6857413808024,209.270833331422));
#35270=CARTESIAN_POINT('Ctrl Pts',(26.787903481163,63.761980950099,209.212499998088));
#35271=CARTESIAN_POINT('Ctrl Pts',(26.787903481163,62.8382205193956,209.154166664755));
#35272=CARTESIAN_POINT('Ctrl Pts',(25.987903481163,62.3763403040439,209.095833331422));
#35273=CARTESIAN_POINT('Ctrl Pts',(25.187903481163,61.9144600886922,209.037499998088));
#35274=CARTESIAN_POINT('Ctrl Pts',(24.387903481163,62.3763403040439,208.979166664755));
#35275=CARTESIAN_POINT('Ctrl Pts',(23.587903481163,62.8382205193956,208.920833331422));
#35276=CARTESIAN_POINT('Ctrl Pts',(23.587903481163,63.761980950099,208.862499998088));
#35277=CARTESIAN_POINT('Ctrl Pts',(23.587903481163,64.6857413808024,208.804166664755));
#35278=CARTESIAN_POINT('Ctrl Pts',(24.387903481163,65.1476215961541,208.745833331422));
#35279=CARTESIAN_POINT('Ctrl Pts',(25.187903481163,65.6095018115058,208.687499998088));
#35280=CARTESIAN_POINT('Ctrl Pts',(25.987903481163,65.1476215961541,208.629166664755));
#35281=CARTESIAN_POINT('Ctrl Pts',(26.787903481163,64.6857413808024,208.570833331422));
#35282=CARTESIAN_POINT('Ctrl Pts',(26.787903481163,63.761980950099,208.512499998088));
#35283=CARTESIAN_POINT('Ctrl Pts',(26.787903481163,62.8382205193956,208.454166664755));
#35284=CARTESIAN_POINT('Ctrl Pts',(25.987903481163,62.3763403040439,208.395833331421));
#35285=CARTESIAN_POINT('Ctrl Pts',(25.187903481163,61.9144600886922,208.337499998088));
#35286=CARTESIAN_POINT('Ctrl Pts',(24.387903481163,62.3763403040439,208.279166664755));
#35287=CARTESIAN_POINT('Ctrl Pts',(23.587903481163,62.8382205193956,208.220833331421));
#35288=CARTESIAN_POINT('Ctrl Pts',(23.587903481163,63.761980950099,208.162499998088));
#35289=CARTESIAN_POINT('Ctrl Pts',(23.587903481163,64.6857413808024,208.104166664755));
#35290=CARTESIAN_POINT('Ctrl Pts',(24.387903481163,65.1476215961541,208.045833331421));
#35291=CARTESIAN_POINT('Ctrl Pts',(25.187903481163,65.6095018115058,207.987499998088));
#35292=CARTESIAN_POINT('Ctrl Pts',(25.987903481163,65.1476215961541,207.929166664755));
#35293=CARTESIAN_POINT('Ctrl Pts',(26.787903481163,64.6857413808024,207.870833331422));
#35294=CARTESIAN_POINT('Ctrl Pts',(26.787903481163,63.761980950099,207.812499998088));
#35295=CARTESIAN_POINT('Ctrl Pts',(26.787903481163,62.8382205193956,207.754166664755));
#35296=CARTESIAN_POINT('Ctrl Pts',(25.987903481163,62.3763403040439,207.695833331422));
#35297=CARTESIAN_POINT('Ctrl Pts',(25.187903481163,61.9144600886922,207.637499998088));
#35298=CARTESIAN_POINT('Ctrl Pts',(24.387903481163,62.3763403040439,207.579166664755));
#35299=CARTESIAN_POINT('Ctrl Pts',(23.587903481163,62.8382205193956,207.520833331422));
#35300=CARTESIAN_POINT('Ctrl Pts',(23.587903481163,63.761980950099,207.462499998088));
#35301=CARTESIAN_POINT('Ctrl Pts',(23.587903481163,64.6857413808024,207.404166664755));
#35302=CARTESIAN_POINT('Ctrl Pts',(24.387903481163,65.1476215961541,207.345833331422));
#35303=CARTESIAN_POINT('Ctrl Pts',(25.187903481163,65.6095018115058,207.287499998088));
#35304=CARTESIAN_POINT('Ctrl Pts',(25.987903481163,65.1476215961541,207.229166664755));
#35305=CARTESIAN_POINT('Ctrl Pts',(26.787903481163,64.6857413808024,207.170833331422));
#35306=CARTESIAN_POINT('Ctrl Pts',(26.787903481163,63.761980950099,207.112499998088));
#35307=CARTESIAN_POINT('Ctrl Pts',(26.787903481163,62.8382205193956,207.054166664755));
#35308=CARTESIAN_POINT('Ctrl Pts',(25.987903481163,62.3763403040439,206.995833331422));
#35309=CARTESIAN_POINT('Ctrl Pts',(25.187903481163,61.9144600886922,206.937499998088));
#35310=CARTESIAN_POINT('Ctrl Pts',(24.387903481163,62.3763403040439,206.879166664755));
#35311=CARTESIAN_POINT('Ctrl Pts',(23.587903481163,62.8382205193956,206.820833331422));
#35312=CARTESIAN_POINT('Ctrl Pts',(23.587903481163,63.761980950099,206.762499998088));
#35313=CARTESIAN_POINT('Ctrl Pts',(23.587903481163,64.6857413808024,206.704166664755));
#35314=CARTESIAN_POINT('Ctrl Pts',(24.387903481163,65.1476215961541,206.645833331421));
#35315=CARTESIAN_POINT('Ctrl Pts',(25.187903481163,65.6095018115058,206.587499998088));
#35316=CARTESIAN_POINT('Ctrl Pts',(25.987903481163,65.1476215961541,206.529166664755));
#35317=CARTESIAN_POINT('Ctrl Pts',(26.787903481163,64.6857413808024,206.470833331422));
#35318=CARTESIAN_POINT('Ctrl Pts',(26.787903481163,63.761980950099,206.412499998088));
#35319=CARTESIAN_POINT('Ctrl Pts',(26.787903481163,62.8382205193956,206.354166664755));
#35320=CARTESIAN_POINT('Ctrl Pts',(25.987903481163,62.3763403040439,206.295833331422));
#35321=CARTESIAN_POINT('Ctrl Pts',(25.187903481163,61.9144600886922,206.237499998088));
#35322=CARTESIAN_POINT('Ctrl Pts',(24.387903481163,62.3763403040439,206.179166664755));
#35323=CARTESIAN_POINT('Ctrl Pts',(23.587903481163,62.8382205193956,206.120833331422));
#35324=CARTESIAN_POINT('Ctrl Pts',(23.587903481163,63.761980950099,206.062499998088));
#35325=CARTESIAN_POINT('Ctrl Pts',(23.587903481163,64.6857413808024,206.004166664755));
#35326=CARTESIAN_POINT('Ctrl Pts',(24.387903481163,65.1476215961541,205.945833331422));
#35327=CARTESIAN_POINT('Ctrl Pts',(25.187903481163,65.6095018115058,205.887499998088));
#35328=CARTESIAN_POINT('Ctrl Pts',(25.987903481163,65.1476215961541,205.829166664755));
#35329=CARTESIAN_POINT('Ctrl Pts',(26.787903481163,64.6857413808024,205.770833331422));
#35330=CARTESIAN_POINT('Ctrl Pts',(26.787903481163,63.761980950099,205.712499998088));
#35331=CARTESIAN_POINT('Ctrl Pts',(26.787903481163,62.8382205193956,205.654166664755));
#35332=CARTESIAN_POINT('Ctrl Pts',(25.987903481163,62.3763403040439,205.595833331421));
#35333=CARTESIAN_POINT('Ctrl Pts',(25.187903481163,61.9144600886922,205.537499998088));
#35334=CARTESIAN_POINT('Ctrl Pts',(24.387903481163,62.3763403040439,205.479166664755));
#35335=CARTESIAN_POINT('Ctrl Pts',(23.587903481163,62.8382205193956,205.420833331422));
#35336=CARTESIAN_POINT('Ctrl Pts',(23.587903481163,63.761980950099,205.362499998088));
#35337=CARTESIAN_POINT('Ctrl Pts',(23.587903481163,64.6857413808024,205.304166664755));
#35338=CARTESIAN_POINT('Ctrl Pts',(24.387903481163,65.1476215961541,205.245833331421));
#35339=CARTESIAN_POINT('Ctrl Pts',(25.187903481163,65.6095018115058,205.187499998088));
#35340=CARTESIAN_POINT('Ctrl Pts',(25.987903481163,65.1476215961541,205.129166664755));
#35341=CARTESIAN_POINT('Ctrl Pts',(26.787903481163,64.6857413808024,205.070833331422));
#35342=CARTESIAN_POINT('Ctrl Pts',(26.787903481163,63.761980950099,205.012499998088));
#35343=CARTESIAN_POINT('Ctrl Pts',(26.787903481163,62.8382205193956,204.954166664755));
#35344=CARTESIAN_POINT('Ctrl Pts',(25.987903481163,62.3763403040439,204.895833331421));
#35345=CARTESIAN_POINT('Ctrl Pts',(25.187903481163,61.9144600886922,204.837499998088));
#35346=CARTESIAN_POINT('Ctrl Pts',(24.387903481163,62.3763403040439,204.779166664755));
#35347=CARTESIAN_POINT('Ctrl Pts',(23.587903481163,62.8382205193956,204.720833331422));
#35348=CARTESIAN_POINT('Ctrl Pts',(23.587903481163,63.761980950099,204.662499998088));
#35349=CARTESIAN_POINT('Ctrl Pts',(23.587903481163,64.6857413808024,204.604166664755));
#35350=CARTESIAN_POINT('Ctrl Pts',(24.387903481163,65.1476215961541,204.545833331422));
#35351=CARTESIAN_POINT('Ctrl Pts',(25.187903481163,65.6095018115058,204.487499998088));
#35352=CARTESIAN_POINT('Ctrl Pts',(25.987903481163,65.1476215961541,204.429166664755));
#35353=CARTESIAN_POINT('Ctrl Pts',(26.787903481163,64.6857413808024,204.370833331422));
#35354=CARTESIAN_POINT('Ctrl Pts',(26.787903481163,63.761980950099,204.312499998088));
#35355=CARTESIAN_POINT('Ctrl Pts',(26.787903481163,62.8382205193956,204.254166664755));
#35356=CARTESIAN_POINT('Ctrl Pts',(25.987903481163,62.3763403040439,204.195833331422));
#35357=CARTESIAN_POINT('Ctrl Pts',(25.187903481163,61.9144600886922,204.137499998088));
#35358=CARTESIAN_POINT('Ctrl Pts',(24.387903481163,62.3763403040439,204.079166664755));
#35359=CARTESIAN_POINT('Ctrl Pts',(23.587903481163,62.8382205193956,204.020833331421));
#35360=CARTESIAN_POINT('Ctrl Pts',(23.587903481163,63.761980950099,203.962499998088));
#35361=CARTESIAN_POINT('Ctrl Pts',(23.587903481163,64.6857413808024,203.904166664755));
#35362=CARTESIAN_POINT('Ctrl Pts',(24.387903481163,65.1476215961541,203.845833331421));
#35363=CARTESIAN_POINT('Ctrl Pts',(25.187903481163,65.6095018115058,203.787499998088));
#35364=CARTESIAN_POINT('Ctrl Pts',(25.987903481163,65.1476215961541,203.729166664755));
#35365=CARTESIAN_POINT('Ctrl Pts',(26.787903481163,64.6857413808024,203.670833331421));
#35366=CARTESIAN_POINT('Ctrl Pts',(26.787903481163,63.761980950099,203.612499998088));
#35367=CARTESIAN_POINT('Ctrl Pts',(26.787903481163,62.8382205193956,203.554166664755));
#35368=CARTESIAN_POINT('Ctrl Pts',(25.987903481163,62.3763403040439,203.495833331421));
#35369=CARTESIAN_POINT('Ctrl Pts',(25.187903481163,61.9144600886922,203.437499998088));
#35370=CARTESIAN_POINT('Ctrl Pts',(24.387903481163,62.3763403040439,203.379166664755));
#35371=CARTESIAN_POINT('Ctrl Pts',(23.587903481163,62.8382205193956,203.320833331422));
#35372=CARTESIAN_POINT('Ctrl Pts',(23.587903481163,63.761980950099,203.262499998088));
#35373=CARTESIAN_POINT('Ctrl Pts',(23.587903481163,64.6857413808024,203.204166664755));
#35374=CARTESIAN_POINT('Ctrl Pts',(24.387903481163,65.1476215961541,203.145833331421));
#35375=CARTESIAN_POINT('Ctrl Pts',(25.187903481163,65.6095018115058,203.087499998088));
#35376=CARTESIAN_POINT('Ctrl Pts',(25.987903481163,65.1476215961541,203.029166664755));
#35377=CARTESIAN_POINT('Ctrl Pts',(26.787903481163,64.6857413808024,202.970833331422));
#35378=CARTESIAN_POINT('Ctrl Pts',(26.787903481163,63.761980950099,202.912499998088));
#35379=CARTESIAN_POINT('Ctrl Pts',(26.409017368663,63.761980950099,212.493749999044));
#35380=CARTESIAN_POINT('Ctrl Pts',(26.409017368663,63.0569705184397,212.435416665711));
#35381=CARTESIAN_POINT('Ctrl Pts',(25.798460424913,62.70446530261,212.377083332377));
#35382=CARTESIAN_POINT('Ctrl Pts',(25.187903481163,62.3519600867804,212.318749999044));
#35383=CARTESIAN_POINT('Ctrl Pts',(24.577346537413,62.70446530261,212.260416665711));
#35384=CARTESIAN_POINT('Ctrl Pts',(23.966789593663,63.0569705184397,212.202083332377));
#35385=CARTESIAN_POINT('Ctrl Pts',(23.966789593663,63.761980950099,212.143749999044));
#35386=CARTESIAN_POINT('Ctrl Pts',(23.966789593663,64.4669913817583,212.085416665711));
#35387=CARTESIAN_POINT('Ctrl Pts',(24.577346537413,64.819496597588,212.027083332377));
#35388=CARTESIAN_POINT('Ctrl Pts',(25.187903481163,65.1720018134176,211.968749999044));
#35389=CARTESIAN_POINT('Ctrl Pts',(25.798460424913,64.819496597588,211.910416665711));
#35390=CARTESIAN_POINT('Ctrl Pts',(26.409017368663,64.4669913817583,211.852083332377));
#35391=CARTESIAN_POINT('Ctrl Pts',(26.409017368663,63.761980950099,211.793749999044));
#35392=CARTESIAN_POINT('Ctrl Pts',(26.409017368663,63.0569705184397,211.735416665711));
#35393=CARTESIAN_POINT('Ctrl Pts',(25.798460424913,62.70446530261,211.677083332377));
#35394=CARTESIAN_POINT('Ctrl Pts',(25.187903481163,62.3519600867804,211.618749999044));
#35395=CARTESIAN_POINT('Ctrl Pts',(24.577346537413,62.70446530261,211.560416665711));
#35396=CARTESIAN_POINT('Ctrl Pts',(23.966789593663,63.0569705184397,211.502083332377));
#35397=CARTESIAN_POINT('Ctrl Pts',(23.966789593663,63.761980950099,211.443749999044));
#35398=CARTESIAN_POINT('Ctrl Pts',(23.966789593663,64.4669913817583,211.385416665711));
#35399=CARTESIAN_POINT('Ctrl Pts',(24.577346537413,64.819496597588,211.327083332377));
#35400=CARTESIAN_POINT('Ctrl Pts',(25.187903481163,65.1720018134176,211.268749999044));
#35401=CARTESIAN_POINT('Ctrl Pts',(25.798460424913,64.819496597588,211.210416665711));
#35402=CARTESIAN_POINT('Ctrl Pts',(26.409017368663,64.4669913817583,211.152083332377));
#35403=CARTESIAN_POINT('Ctrl Pts',(26.409017368663,63.761980950099,211.093749999044));
#35404=CARTESIAN_POINT('Ctrl Pts',(26.409017368663,63.0569705184397,211.035416665711));
#35405=CARTESIAN_POINT('Ctrl Pts',(25.798460424913,62.70446530261,210.977083332377));
#35406=CARTESIAN_POINT('Ctrl Pts',(25.187903481163,62.3519600867804,210.918749999044));
#35407=CARTESIAN_POINT('Ctrl Pts',(24.577346537413,62.70446530261,210.860416665711));
#35408=CARTESIAN_POINT('Ctrl Pts',(23.966789593663,63.0569705184397,210.802083332377));
#35409=CARTESIAN_POINT('Ctrl Pts',(23.966789593663,63.761980950099,210.743749999044));
#35410=CARTESIAN_POINT('Ctrl Pts',(23.966789593663,64.4669913817583,210.685416665711));
#35411=CARTESIAN_POINT('Ctrl Pts',(24.577346537413,64.819496597588,210.627083332377));
#35412=CARTESIAN_POINT('Ctrl Pts',(25.187903481163,65.1720018134176,210.568749999044));
#35413=CARTESIAN_POINT('Ctrl Pts',(25.798460424913,64.819496597588,210.510416665711));
#35414=CARTESIAN_POINT('Ctrl Pts',(26.409017368663,64.4669913817583,210.452083332377));
#35415=CARTESIAN_POINT('Ctrl Pts',(26.409017368663,63.761980950099,210.393749999044));
#35416=CARTESIAN_POINT('Ctrl Pts',(26.409017368663,63.0569705184397,210.335416665711));
#35417=CARTESIAN_POINT('Ctrl Pts',(25.798460424913,62.70446530261,210.277083332377));
#35418=CARTESIAN_POINT('Ctrl Pts',(25.187903481163,62.3519600867804,210.218749999044));
#35419=CARTESIAN_POINT('Ctrl Pts',(24.577346537413,62.70446530261,210.160416665711));
#35420=CARTESIAN_POINT('Ctrl Pts',(23.966789593663,63.0569705184397,210.102083332377));
#35421=CARTESIAN_POINT('Ctrl Pts',(23.966789593663,63.761980950099,210.043749999044));
#35422=CARTESIAN_POINT('Ctrl Pts',(23.966789593663,64.4669913817583,209.985416665711));
#35423=CARTESIAN_POINT('Ctrl Pts',(24.577346537413,64.819496597588,209.927083332377));
#35424=CARTESIAN_POINT('Ctrl Pts',(25.187903481163,65.1720018134176,209.868749999044));
#35425=CARTESIAN_POINT('Ctrl Pts',(25.798460424913,64.819496597588,209.810416665711));
#35426=CARTESIAN_POINT('Ctrl Pts',(26.409017368663,64.4669913817583,209.752083332377));
#35427=CARTESIAN_POINT('Ctrl Pts',(26.409017368663,63.761980950099,209.693749999044));
#35428=CARTESIAN_POINT('Ctrl Pts',(26.409017368663,63.0569705184397,209.635416665711));
#35429=CARTESIAN_POINT('Ctrl Pts',(25.798460424913,62.70446530261,209.577083332377));
#35430=CARTESIAN_POINT('Ctrl Pts',(25.187903481163,62.3519600867804,209.518749999044));
#35431=CARTESIAN_POINT('Ctrl Pts',(24.577346537413,62.70446530261,209.460416665711));
#35432=CARTESIAN_POINT('Ctrl Pts',(23.966789593663,63.0569705184397,209.402083332377));
#35433=CARTESIAN_POINT('Ctrl Pts',(23.966789593663,63.761980950099,209.343749999044));
#35434=CARTESIAN_POINT('Ctrl Pts',(23.966789593663,64.4669913817583,209.285416665711));
#35435=CARTESIAN_POINT('Ctrl Pts',(24.577346537413,64.819496597588,209.227083332377));
#35436=CARTESIAN_POINT('Ctrl Pts',(25.187903481163,65.1720018134176,209.168749999044));
#35437=CARTESIAN_POINT('Ctrl Pts',(25.798460424913,64.819496597588,209.110416665711));
#35438=CARTESIAN_POINT('Ctrl Pts',(26.409017368663,64.4669913817583,209.052083332377));
#35439=CARTESIAN_POINT('Ctrl Pts',(26.409017368663,63.761980950099,208.993749999044));
#35440=CARTESIAN_POINT('Ctrl Pts',(26.409017368663,63.0569705184397,208.935416665711));
#35441=CARTESIAN_POINT('Ctrl Pts',(25.798460424913,62.70446530261,208.877083332377));
#35442=CARTESIAN_POINT('Ctrl Pts',(25.187903481163,62.3519600867804,208.818749999044));
#35443=CARTESIAN_POINT('Ctrl Pts',(24.577346537413,62.70446530261,208.760416665711));
#35444=CARTESIAN_POINT('Ctrl Pts',(23.966789593663,63.0569705184397,208.702083332377));
#35445=CARTESIAN_POINT('Ctrl Pts',(23.966789593663,63.761980950099,208.643749999044));
#35446=CARTESIAN_POINT('Ctrl Pts',(23.966789593663,64.4669913817583,208.585416665711));
#35447=CARTESIAN_POINT('Ctrl Pts',(24.577346537413,64.819496597588,208.527083332377));
#35448=CARTESIAN_POINT('Ctrl Pts',(25.187903481163,65.1720018134176,208.468749999044));
#35449=CARTESIAN_POINT('Ctrl Pts',(25.798460424913,64.819496597588,208.410416665711));
#35450=CARTESIAN_POINT('Ctrl Pts',(26.409017368663,64.4669913817583,208.352083332377));
#35451=CARTESIAN_POINT('Ctrl Pts',(26.409017368663,63.761980950099,208.293749999044));
#35452=CARTESIAN_POINT('Ctrl Pts',(26.409017368663,63.0569705184397,208.235416665711));
#35453=CARTESIAN_POINT('Ctrl Pts',(25.798460424913,62.70446530261,208.177083332377));
#35454=CARTESIAN_POINT('Ctrl Pts',(25.187903481163,62.3519600867804,208.118749999044));
#35455=CARTESIAN_POINT('Ctrl Pts',(24.577346537413,62.70446530261,208.060416665711));
#35456=CARTESIAN_POINT('Ctrl Pts',(23.966789593663,63.0569705184397,208.002083332377));
#35457=CARTESIAN_POINT('Ctrl Pts',(23.966789593663,63.761980950099,207.943749999044));
#35458=CARTESIAN_POINT('Ctrl Pts',(23.966789593663,64.4669913817583,207.885416665711));
#35459=CARTESIAN_POINT('Ctrl Pts',(24.577346537413,64.819496597588,207.827083332377));
#35460=CARTESIAN_POINT('Ctrl Pts',(25.187903481163,65.1720018134176,207.768749999044));
#35461=CARTESIAN_POINT('Ctrl Pts',(25.798460424913,64.819496597588,207.710416665711));
#35462=CARTESIAN_POINT('Ctrl Pts',(26.409017368663,64.4669913817583,207.652083332377));
#35463=CARTESIAN_POINT('Ctrl Pts',(26.409017368663,63.761980950099,207.593749999044));
#35464=CARTESIAN_POINT('Ctrl Pts',(26.409017368663,63.0569705184397,207.535416665711));
#35465=CARTESIAN_POINT('Ctrl Pts',(25.798460424913,62.70446530261,207.477083332377));
#35466=CARTESIAN_POINT('Ctrl Pts',(25.187903481163,62.3519600867804,207.418749999044));
#35467=CARTESIAN_POINT('Ctrl Pts',(24.577346537413,62.70446530261,207.360416665711));
#35468=CARTESIAN_POINT('Ctrl Pts',(23.966789593663,63.0569705184397,207.302083332377));
#35469=CARTESIAN_POINT('Ctrl Pts',(23.966789593663,63.761980950099,207.243749999044));
#35470=CARTESIAN_POINT('Ctrl Pts',(23.966789593663,64.4669913817583,207.185416665711));
#35471=CARTESIAN_POINT('Ctrl Pts',(24.577346537413,64.819496597588,207.127083332377));
#35472=CARTESIAN_POINT('Ctrl Pts',(25.187903481163,65.1720018134176,207.068749999044));
#35473=CARTESIAN_POINT('Ctrl Pts',(25.798460424913,64.819496597588,207.010416665711));
#35474=CARTESIAN_POINT('Ctrl Pts',(26.409017368663,64.4669913817583,206.952083332377));
#35475=CARTESIAN_POINT('Ctrl Pts',(26.409017368663,63.761980950099,206.893749999044));
#35476=CARTESIAN_POINT('Ctrl Pts',(26.409017368663,63.0569705184397,206.835416665711));
#35477=CARTESIAN_POINT('Ctrl Pts',(25.798460424913,62.70446530261,206.777083332377));
#35478=CARTESIAN_POINT('Ctrl Pts',(25.187903481163,62.3519600867804,206.718749999044));
#35479=CARTESIAN_POINT('Ctrl Pts',(24.577346537413,62.70446530261,206.660416665711));
#35480=CARTESIAN_POINT('Ctrl Pts',(23.966789593663,63.0569705184397,206.602083332377));
#35481=CARTESIAN_POINT('Ctrl Pts',(23.966789593663,63.761980950099,206.543749999044));
#35482=CARTESIAN_POINT('Ctrl Pts',(23.966789593663,64.4669913817583,206.485416665711));
#35483=CARTESIAN_POINT('Ctrl Pts',(24.577346537413,64.819496597588,206.427083332377));
#35484=CARTESIAN_POINT('Ctrl Pts',(25.187903481163,65.1720018134176,206.368749999044));
#35485=CARTESIAN_POINT('Ctrl Pts',(25.798460424913,64.819496597588,206.310416665711));
#35486=CARTESIAN_POINT('Ctrl Pts',(26.409017368663,64.4669913817583,206.252083332377));
#35487=CARTESIAN_POINT('Ctrl Pts',(26.409017368663,63.761980950099,206.193749999044));
#35488=CARTESIAN_POINT('Ctrl Pts',(26.409017368663,63.0569705184397,206.135416665711));
#35489=CARTESIAN_POINT('Ctrl Pts',(25.798460424913,62.70446530261,206.077083332377));
#35490=CARTESIAN_POINT('Ctrl Pts',(25.187903481163,62.3519600867804,206.018749999044));
#35491=CARTESIAN_POINT('Ctrl Pts',(24.577346537413,62.70446530261,205.960416665711));
#35492=CARTESIAN_POINT('Ctrl Pts',(23.966789593663,63.0569705184397,205.902083332377));
#35493=CARTESIAN_POINT('Ctrl Pts',(23.966789593663,63.761980950099,205.843749999044));
#35494=CARTESIAN_POINT('Ctrl Pts',(23.966789593663,64.4669913817583,205.785416665711));
#35495=CARTESIAN_POINT('Ctrl Pts',(24.577346537413,64.819496597588,205.727083332377));
#35496=CARTESIAN_POINT('Ctrl Pts',(25.187903481163,65.1720018134176,205.668749999044));
#35497=CARTESIAN_POINT('Ctrl Pts',(25.798460424913,64.819496597588,205.610416665711));
#35498=CARTESIAN_POINT('Ctrl Pts',(26.409017368663,64.4669913817583,205.552083332377));
#35499=CARTESIAN_POINT('Ctrl Pts',(26.409017368663,63.761980950099,205.493749999044));
#35500=CARTESIAN_POINT('Ctrl Pts',(26.409017368663,63.0569705184397,205.435416665711));
#35501=CARTESIAN_POINT('Ctrl Pts',(25.798460424913,62.70446530261,205.377083332377));
#35502=CARTESIAN_POINT('Ctrl Pts',(25.187903481163,62.3519600867804,205.318749999044));
#35503=CARTESIAN_POINT('Ctrl Pts',(24.577346537413,62.70446530261,205.260416665711));
#35504=CARTESIAN_POINT('Ctrl Pts',(23.966789593663,63.0569705184397,205.202083332377));
#35505=CARTESIAN_POINT('Ctrl Pts',(23.966789593663,63.761980950099,205.143749999044));
#35506=CARTESIAN_POINT('Ctrl Pts',(23.966789593663,64.4669913817583,205.085416665711));
#35507=CARTESIAN_POINT('Ctrl Pts',(24.577346537413,64.819496597588,205.027083332377));
#35508=CARTESIAN_POINT('Ctrl Pts',(25.187903481163,65.1720018134176,204.968749999044));
#35509=CARTESIAN_POINT('Ctrl Pts',(25.798460424913,64.819496597588,204.910416665711));
#35510=CARTESIAN_POINT('Ctrl Pts',(26.409017368663,64.4669913817583,204.852083332377));
#35511=CARTESIAN_POINT('Ctrl Pts',(26.409017368663,63.761980950099,204.793749999044));
#35512=CARTESIAN_POINT('Ctrl Pts',(26.409017368663,63.0569705184397,204.735416665711));
#35513=CARTESIAN_POINT('Ctrl Pts',(25.798460424913,62.70446530261,204.677083332377));
#35514=CARTESIAN_POINT('Ctrl Pts',(25.187903481163,62.3519600867804,204.618749999044));
#35515=CARTESIAN_POINT('Ctrl Pts',(24.577346537413,62.70446530261,204.560416665711));
#35516=CARTESIAN_POINT('Ctrl Pts',(23.966789593663,63.0569705184397,204.502083332377));
#35517=CARTESIAN_POINT('Ctrl Pts',(23.966789593663,63.761980950099,204.443749999044));
#35518=CARTESIAN_POINT('Ctrl Pts',(23.966789593663,64.4669913817583,204.385416665711));
#35519=CARTESIAN_POINT('Ctrl Pts',(24.577346537413,64.819496597588,204.327083332377));
#35520=CARTESIAN_POINT('Ctrl Pts',(25.187903481163,65.1720018134176,204.268749999044));
#35521=CARTESIAN_POINT('Ctrl Pts',(25.798460424913,64.819496597588,204.210416665711));
#35522=CARTESIAN_POINT('Ctrl Pts',(26.409017368663,64.4669913817583,204.152083332377));
#35523=CARTESIAN_POINT('Ctrl Pts',(26.409017368663,63.761980950099,204.093749999044));
#35524=CARTESIAN_POINT('Ctrl Pts',(26.409017368663,63.0569705184397,204.035416665711));
#35525=CARTESIAN_POINT('Ctrl Pts',(25.798460424913,62.70446530261,203.977083332377));
#35526=CARTESIAN_POINT('Ctrl Pts',(25.187903481163,62.3519600867804,203.918749999044));
#35527=CARTESIAN_POINT('Ctrl Pts',(24.577346537413,62.70446530261,203.860416665711));
#35528=CARTESIAN_POINT('Ctrl Pts',(23.966789593663,63.0569705184397,203.802083332377));
#35529=CARTESIAN_POINT('Ctrl Pts',(23.966789593663,63.761980950099,203.743749999044));
#35530=CARTESIAN_POINT('Ctrl Pts',(23.966789593663,64.4669913817583,203.685416665711));
#35531=CARTESIAN_POINT('Ctrl Pts',(24.577346537413,64.819496597588,203.627083332377));
#35532=CARTESIAN_POINT('Ctrl Pts',(25.187903481163,65.1720018134176,203.568749999044));
#35533=CARTESIAN_POINT('Ctrl Pts',(25.798460424913,64.819496597588,203.510416665711));
#35534=CARTESIAN_POINT('Ctrl Pts',(26.409017368663,64.4669913817583,203.452083332377));
#35535=CARTESIAN_POINT('Ctrl Pts',(26.409017368663,63.761980950099,203.393749999044));
#35536=CARTESIAN_POINT('Ctrl Pts',(26.409017368663,63.0569705184397,203.335416665711));
#35537=CARTESIAN_POINT('Ctrl Pts',(25.798460424913,62.70446530261,203.277083332377));
#35538=CARTESIAN_POINT('Ctrl Pts',(25.187903481163,62.3519600867804,203.218749999044));
#35539=CARTESIAN_POINT('Ctrl Pts',(24.577346537413,62.70446530261,203.160416665711));
#35540=CARTESIAN_POINT('Ctrl Pts',(23.966789593663,63.0569705184397,203.102083332377));
#35541=CARTESIAN_POINT('Ctrl Pts',(23.966789593663,63.761980950099,203.043749999044));
#35542=CARTESIAN_POINT('Ctrl Pts',(23.966789593663,64.4669913817583,202.985416665711));
#35543=CARTESIAN_POINT('Ctrl Pts',(24.577346537413,64.819496597588,202.927083332377));
#35544=CARTESIAN_POINT('Ctrl Pts',(25.187903481163,65.1720018134176,202.868749999044));
#35545=CARTESIAN_POINT('Ctrl Pts',(25.798460424913,64.819496597588,202.810416665711));
#35546=CARTESIAN_POINT('Ctrl Pts',(26.409017368663,64.4669913817583,202.752083332377));
#35547=CARTESIAN_POINT('Ctrl Pts',(26.409017368663,63.761980950099,202.693749999044));
#35548=CARTESIAN_POINT('',(26.598460424913,63.761980950099,212.603124998566));
#35549=CARTESIAN_POINT('Ctrl Pts',(23.966789593663,63.761980950099,212.143749999044));
#35550=CARTESIAN_POINT('Ctrl Pts',(23.966789593663,64.4669913817583,212.085416665711));
#35551=CARTESIAN_POINT('Ctrl Pts',(24.577346537413,64.819496597588,212.027083332377));
#35552=CARTESIAN_POINT('Ctrl Pts',(25.187903481163,65.1720018134176,211.968749999044));
#35553=CARTESIAN_POINT('Ctrl Pts',(25.798460424913,64.819496597588,211.910416665711));
#35554=CARTESIAN_POINT('Ctrl Pts',(26.409017368663,64.4669913817583,211.852083332377));
#35555=CARTESIAN_POINT('Ctrl Pts',(26.409017368663,63.761980950099,211.793749999044));
#35556=CARTESIAN_POINT('Ctrl Pts',(26.409017368663,63.0569705184397,211.735416665711));
#35557=CARTESIAN_POINT('Ctrl Pts',(25.798460424913,62.70446530261,211.677083332377));
#35558=CARTESIAN_POINT('Ctrl Pts',(25.187903481163,62.3519600867804,211.618749999044));
#35559=CARTESIAN_POINT('Ctrl Pts',(24.577346537413,62.70446530261,211.560416665711));
#35560=CARTESIAN_POINT('Ctrl Pts',(23.966789593663,63.0569705184397,211.502083332377));
#35561=CARTESIAN_POINT('Ctrl Pts',(23.966789593663,63.761980950099,211.443749999044));
#35562=CARTESIAN_POINT('',(26.598460424913,63.761980950099,202.803124998566));
#35563=CARTESIAN_POINT('Ctrl Pts',(26.787903481163,63.761980950099,211.312499998088));
#35564=CARTESIAN_POINT('Ctrl Pts',(26.787903481163,63.8741171554749,211.31958113994));
#35565=CARTESIAN_POINT('Ctrl Pts',(26.7761195543677,63.9861700545367,211.327086643522));
#35566=CARTESIAN_POINT('Ctrl Pts',(26.7081426976078,64.3042786309023,211.349652786821));
#35567=CARTESIAN_POINT('Ctrl Pts',(26.6227037454562,64.5012658582677,211.365207036137));
#35568=CARTESIAN_POINT('Ctrl Pts',(26.3844510384125,64.8437047737,211.395517557749));
#35569=CARTESIAN_POINT('Ctrl Pts',(26.2364517101797,64.9877218095493,211.410007709105));
#35570=CARTESIAN_POINT('Ctrl Pts',(25.8878489096898,65.2163196275864,211.43715260937));
#35571=CARTESIAN_POINT('Ctrl Pts',(25.6889946080725,65.2962516439341,211.450962103418));
#35572=CARTESIAN_POINT('Ctrl Pts',(25.2738293345874,65.3734083731304,211.481234571276));
#35573=CARTESIAN_POINT('Ctrl Pts',(25.0618583522795,65.3707681781366,211.496690788736));
#35574=CARTESIAN_POINT('Ctrl Pts',(24.658014157987,65.2852538654097,211.526137761236));
#35575=CARTESIAN_POINT('Ctrl Pts',(24.4694561743753,65.2059105467147,211.539179243819));
#35576=CARTESIAN_POINT('Ctrl Pts',(24.1240235923046,64.9757575818482,211.566306767127));
#35577=CARTESIAN_POINT('Ctrl Pts',(23.9725451147546,64.8240328301937,211.581410486883));
#35578=CARTESIAN_POINT('Ctrl Pts',(23.7403019497449,64.4743774588544,211.611957613098));
#35579=CARTESIAN_POINT('Ctrl Pts',(23.6601932823326,64.2808084410836,211.627101677091));
#35580=CARTESIAN_POINT('Ctrl Pts',(23.5789696508475,63.8767726017523,211.655576883513));
#35581=CARTESIAN_POINT('Ctrl Pts',(23.5774814489119,63.6704113360506,211.667902437369));
#35582=CARTESIAN_POINT('Ctrl Pts',(23.6538984231461,63.259704709123,211.696623645877));
#35583=CARTESIAN_POINT('Ctrl Pts',(23.7343932347138,63.0600292555202,211.712167395334));
#35584=CARTESIAN_POINT('Ctrl Pts',(23.9644062950721,62.7107366852901,211.742610305599));
#35585=CARTESIAN_POINT('Ctrl Pts',(24.1091112487229,62.5626871708893,211.757234991236));
#35586=CARTESIAN_POINT('Ctrl Pts',(24.4509406583139,62.326305836117,211.784624456026));
#35587=CARTESIAN_POINT('Ctrl Pts',(24.6459233339367,62.241925135792,211.797980612353));
#35588=CARTESIAN_POINT('Ctrl Pts',(25.0575582231217,62.1534622407589,211.827995656356));
#35589=CARTESIAN_POINT('Ctrl Pts',(25.2701052598562,62.1502853772832,211.843493877785));
#35590=CARTESIAN_POINT('Ctrl Pts',(25.6768194963091,62.2250449198287,211.873150124193));
#35591=CARTESIAN_POINT('Ctrl Pts',(25.8675789383445,62.2993855707684,211.886586985822));
#35592=CARTESIAN_POINT('Ctrl Pts',(26.2190795897561,62.5203062212873,211.91335274154));
#35593=CARTESIAN_POINT('Ctrl Pts',(26.3745177920632,62.6679156807696,211.928340955085));
#35594=CARTESIAN_POINT('Ctrl Pts',(26.6162914621394,63.0116546221704,211.958861938772));
#35595=CARTESIAN_POINT('Ctrl Pts',(26.7016619877479,63.2035596364255,211.974092763374));
#35596=CARTESIAN_POINT('Ctrl Pts',(26.7745478971648,63.523360725262,211.996944760797));
#35597=CARTESIAN_POINT('Ctrl Pts',(26.787903481163,63.6425978678265,212.004961232732));
#35598=CARTESIAN_POINT('Ctrl Pts',(26.787903481163,63.7619809500991,212.012499998088));
#35599=CARTESIAN_POINT('Origin',(25.1879034811629,63.761980950099,212.406249999044));
#35600=CARTESIAN_POINT('Ctrl Pts',(23.966789593663,63.761980950099,211.968749999044));
#35601=CARTESIAN_POINT('Ctrl Pts',(23.966789593663,64.4669913817583,211.910416665711));
#35602=CARTESIAN_POINT('Ctrl Pts',(24.577346537413,64.819496597588,211.852083332377));
#35603=CARTESIAN_POINT('Ctrl Pts',(25.187903481163,65.1720018134176,211.793749999044));
#35604=CARTESIAN_POINT('Ctrl Pts',(25.798460424913,64.819496597588,211.735416665711));
#35605=CARTESIAN_POINT('Ctrl Pts',(26.409017368663,64.4669913817583,211.677083332377));
#35606=CARTESIAN_POINT('Ctrl Pts',(26.409017368663,63.761980950099,211.618749999044));
#35607=CARTESIAN_POINT('Ctrl Pts',(26.409017368663,63.0569705184397,211.560416665711));
#35608=CARTESIAN_POINT('Ctrl Pts',(25.798460424913,62.70446530261,211.502083332377));
#35609=CARTESIAN_POINT('Ctrl Pts',(25.187903481163,62.3519600867804,211.443749999044));
#35610=CARTESIAN_POINT('Ctrl Pts',(24.577346537413,62.70446530261,211.385416665711));
#35611=CARTESIAN_POINT('Ctrl Pts',(23.966789593663,63.0569705184397,211.327083332377));
#35612=CARTESIAN_POINT('Ctrl Pts',(23.966789593663,63.761980950099,211.268749999044));
#35613=CARTESIAN_POINT('Ctrl Pts',(26.409017368663,63.761980950099,212.318749999044));
#35614=CARTESIAN_POINT('Ctrl Pts',(26.409017368663,63.0569705184397,212.260416665711));
#35615=CARTESIAN_POINT('Ctrl Pts',(25.798460424913,62.70446530261,212.202083332377));
#35616=CARTESIAN_POINT('Ctrl Pts',(25.187903481163,62.3519600867804,212.143749999044));
#35617=CARTESIAN_POINT('Ctrl Pts',(24.577346537413,62.70446530261,212.085416665711));
#35618=CARTESIAN_POINT('Ctrl Pts',(23.966789593663,63.0569705184397,212.027083332377));
#35619=CARTESIAN_POINT('Ctrl Pts',(23.966789593663,63.761980950099,211.968749999044));
#35620=CARTESIAN_POINT('Ctrl Pts',(23.966789593663,64.4669913817583,211.910416665711));
#35621=CARTESIAN_POINT('Ctrl Pts',(24.577346537413,64.819496597588,211.852083332377));
#35622=CARTESIAN_POINT('Ctrl Pts',(25.187903481163,65.1720018134176,211.793749999044));
#35623=CARTESIAN_POINT('Ctrl Pts',(25.798460424913,64.819496597588,211.735416665711));
#35624=CARTESIAN_POINT('Ctrl Pts',(26.409017368663,64.4669913817583,211.677083332377));
#35625=CARTESIAN_POINT('Ctrl Pts',(26.409017368663,63.761980950099,211.618749999044));
#35626=CARTESIAN_POINT('Ctrl Pts',(26.409017368663,63.0569705184397,211.560416665711));
#35627=CARTESIAN_POINT('Ctrl Pts',(25.798460424913,62.70446530261,211.502083332377));
#35628=CARTESIAN_POINT('Ctrl Pts',(25.187903481163,62.3519600867804,211.443749999044));
#35629=CARTESIAN_POINT('Ctrl Pts',(24.577346537413,62.70446530261,211.385416665711));
#35630=CARTESIAN_POINT('Ctrl Pts',(23.966789593663,63.0569705184397,211.327083332377));
#35631=CARTESIAN_POINT('Ctrl Pts',(23.966789593663,63.761980950099,211.268749999044));
#35632=CARTESIAN_POINT('Ctrl Pts',(23.966789593663,64.4669913817583,211.210416665711));
#35633=CARTESIAN_POINT('Ctrl Pts',(24.577346537413,64.819496597588,211.152083332377));
#35634=CARTESIAN_POINT('Ctrl Pts',(25.187903481163,65.1720018134176,211.093749999044));
#35635=CARTESIAN_POINT('Ctrl Pts',(25.798460424913,64.819496597588,211.035416665711));
#35636=CARTESIAN_POINT('Ctrl Pts',(26.409017368663,64.4669913817583,210.977083332377));
#35637=CARTESIAN_POINT('Ctrl Pts',(26.409017368663,63.761980950099,210.918749999044));
#35638=CARTESIAN_POINT('Ctrl Pts',(26.409017368663,63.0569705184397,210.860416665711));
#35639=CARTESIAN_POINT('Ctrl Pts',(25.798460424913,62.70446530261,210.802083332377));
#35640=CARTESIAN_POINT('Ctrl Pts',(25.187903481163,62.3519600867804,210.743749999044));
#35641=CARTESIAN_POINT('Ctrl Pts',(24.577346537413,62.70446530261,210.685416665711));
#35642=CARTESIAN_POINT('Ctrl Pts',(23.966789593663,63.0569705184397,210.627083332377));
#35643=CARTESIAN_POINT('Ctrl Pts',(23.966789593663,63.761980950099,210.568749999044));
#35644=CARTESIAN_POINT('Ctrl Pts',(23.966789593663,64.4669913817583,210.510416665711));
#35645=CARTESIAN_POINT('Ctrl Pts',(24.577346537413,64.819496597588,210.452083332377));
#35646=CARTESIAN_POINT('Ctrl Pts',(25.187903481163,65.1720018134176,210.393749999044));
#35647=CARTESIAN_POINT('Ctrl Pts',(25.798460424913,64.819496597588,210.335416665711));
#35648=CARTESIAN_POINT('Ctrl Pts',(26.409017368663,64.4669913817583,210.277083332377));
#35649=CARTESIAN_POINT('Ctrl Pts',(26.409017368663,63.761980950099,210.218749999044));
#35650=CARTESIAN_POINT('Ctrl Pts',(26.409017368663,63.0569705184397,210.160416665711));
#35651=CARTESIAN_POINT('Ctrl Pts',(25.798460424913,62.70446530261,210.102083332377));
#35652=CARTESIAN_POINT('Ctrl Pts',(25.187903481163,62.3519600867804,210.043749999044));
#35653=CARTESIAN_POINT('Ctrl Pts',(24.577346537413,62.70446530261,209.985416665711));
#35654=CARTESIAN_POINT('Ctrl Pts',(23.966789593663,63.0569705184397,209.927083332377));
#35655=CARTESIAN_POINT('Ctrl Pts',(23.966789593663,63.761980950099,209.868749999044));
#35656=CARTESIAN_POINT('Ctrl Pts',(23.966789593663,64.4669913817583,209.810416665711));
#35657=CARTESIAN_POINT('Ctrl Pts',(24.577346537413,64.819496597588,209.752083332377));
#35658=CARTESIAN_POINT('Ctrl Pts',(25.187903481163,65.1720018134176,209.693749999044));
#35659=CARTESIAN_POINT('Ctrl Pts',(25.798460424913,64.819496597588,209.635416665711));
#35660=CARTESIAN_POINT('Ctrl Pts',(26.409017368663,64.4669913817583,209.577083332377));
#35661=CARTESIAN_POINT('Ctrl Pts',(26.409017368663,63.761980950099,209.518749999044));
#35662=CARTESIAN_POINT('Ctrl Pts',(26.409017368663,63.0569705184397,209.460416665711));
#35663=CARTESIAN_POINT('Ctrl Pts',(25.798460424913,62.70446530261,209.402083332377));
#35664=CARTESIAN_POINT('Ctrl Pts',(25.187903481163,62.3519600867804,209.343749999044));
#35665=CARTESIAN_POINT('Ctrl Pts',(24.577346537413,62.70446530261,209.285416665711));
#35666=CARTESIAN_POINT('Ctrl Pts',(23.966789593663,63.0569705184397,209.227083332377));
#35667=CARTESIAN_POINT('Ctrl Pts',(23.966789593663,63.761980950099,209.168749999044));
#35668=CARTESIAN_POINT('Ctrl Pts',(23.966789593663,64.4669913817583,209.110416665711));
#35669=CARTESIAN_POINT('Ctrl Pts',(24.577346537413,64.819496597588,209.052083332377));
#35670=CARTESIAN_POINT('Ctrl Pts',(25.187903481163,65.1720018134176,208.993749999044));
#35671=CARTESIAN_POINT('Ctrl Pts',(25.798460424913,64.819496597588,208.935416665711));
#35672=CARTESIAN_POINT('Ctrl Pts',(26.409017368663,64.4669913817583,208.877083332377));
#35673=CARTESIAN_POINT('Ctrl Pts',(26.409017368663,63.761980950099,208.818749999044));
#35674=CARTESIAN_POINT('Ctrl Pts',(26.409017368663,63.0569705184397,208.760416665711));
#35675=CARTESIAN_POINT('Ctrl Pts',(25.798460424913,62.70446530261,208.702083332377));
#35676=CARTESIAN_POINT('Ctrl Pts',(25.187903481163,62.3519600867804,208.643749999044));
#35677=CARTESIAN_POINT('Ctrl Pts',(24.577346537413,62.70446530261,208.585416665711));
#35678=CARTESIAN_POINT('Ctrl Pts',(23.966789593663,63.0569705184397,208.527083332377));
#35679=CARTESIAN_POINT('Ctrl Pts',(23.966789593663,63.761980950099,208.468749999044));
#35680=CARTESIAN_POINT('Ctrl Pts',(23.966789593663,64.4669913817583,208.410416665711));
#35681=CARTESIAN_POINT('Ctrl Pts',(24.577346537413,64.819496597588,208.352083332377));
#35682=CARTESIAN_POINT('Ctrl Pts',(25.187903481163,65.1720018134176,208.293749999044));
#35683=CARTESIAN_POINT('Ctrl Pts',(25.798460424913,64.819496597588,208.235416665711));
#35684=CARTESIAN_POINT('Ctrl Pts',(26.409017368663,64.4669913817583,208.177083332377));
#35685=CARTESIAN_POINT('Ctrl Pts',(26.409017368663,63.761980950099,208.118749999044));
#35686=CARTESIAN_POINT('Ctrl Pts',(26.409017368663,63.0569705184397,208.060416665711));
#35687=CARTESIAN_POINT('Ctrl Pts',(25.798460424913,62.70446530261,208.002083332377));
#35688=CARTESIAN_POINT('Ctrl Pts',(25.187903481163,62.3519600867804,207.943749999044));
#35689=CARTESIAN_POINT('Ctrl Pts',(24.577346537413,62.70446530261,207.885416665711));
#35690=CARTESIAN_POINT('Ctrl Pts',(23.966789593663,63.0569705184397,207.827083332377));
#35691=CARTESIAN_POINT('Ctrl Pts',(23.966789593663,63.761980950099,207.768749999044));
#35692=CARTESIAN_POINT('Ctrl Pts',(23.966789593663,64.4669913817583,207.710416665711));
#35693=CARTESIAN_POINT('Ctrl Pts',(24.577346537413,64.819496597588,207.652083332377));
#35694=CARTESIAN_POINT('Ctrl Pts',(25.187903481163,65.1720018134176,207.593749999044));
#35695=CARTESIAN_POINT('Ctrl Pts',(25.798460424913,64.819496597588,207.535416665711));
#35696=CARTESIAN_POINT('Ctrl Pts',(26.409017368663,64.4669913817583,207.477083332377));
#35697=CARTESIAN_POINT('Ctrl Pts',(26.409017368663,63.761980950099,207.418749999044));
#35698=CARTESIAN_POINT('Ctrl Pts',(26.409017368663,63.0569705184397,207.360416665711));
#35699=CARTESIAN_POINT('Ctrl Pts',(25.798460424913,62.70446530261,207.302083332377));
#35700=CARTESIAN_POINT('Ctrl Pts',(25.187903481163,62.3519600867804,207.243749999044));
#35701=CARTESIAN_POINT('Ctrl Pts',(24.577346537413,62.70446530261,207.185416665711));
#35702=CARTESIAN_POINT('Ctrl Pts',(23.966789593663,63.0569705184397,207.127083332377));
#35703=CARTESIAN_POINT('Ctrl Pts',(23.966789593663,63.761980950099,207.068749999044));
#35704=CARTESIAN_POINT('Ctrl Pts',(23.966789593663,64.4669913817583,207.010416665711));
#35705=CARTESIAN_POINT('Ctrl Pts',(24.577346537413,64.819496597588,206.952083332377));
#35706=CARTESIAN_POINT('Ctrl Pts',(25.187903481163,65.1720018134176,206.893749999044));
#35707=CARTESIAN_POINT('Ctrl Pts',(25.798460424913,64.819496597588,206.835416665711));
#35708=CARTESIAN_POINT('Ctrl Pts',(26.409017368663,64.4669913817583,206.777083332377));
#35709=CARTESIAN_POINT('Ctrl Pts',(26.409017368663,63.761980950099,206.718749999044));
#35710=CARTESIAN_POINT('Ctrl Pts',(26.409017368663,63.0569705184397,206.660416665711));
#35711=CARTESIAN_POINT('Ctrl Pts',(25.798460424913,62.70446530261,206.602083332377));
#35712=CARTESIAN_POINT('Ctrl Pts',(25.187903481163,62.3519600867804,206.543749999044));
#35713=CARTESIAN_POINT('Ctrl Pts',(24.577346537413,62.70446530261,206.485416665711));
#35714=CARTESIAN_POINT('Ctrl Pts',(23.966789593663,63.0569705184397,206.427083332377));
#35715=CARTESIAN_POINT('Ctrl Pts',(23.966789593663,63.761980950099,206.368749999044));
#35716=CARTESIAN_POINT('Ctrl Pts',(23.966789593663,64.4669913817583,206.310416665711));
#35717=CARTESIAN_POINT('Ctrl Pts',(24.577346537413,64.819496597588,206.252083332377));
#35718=CARTESIAN_POINT('Ctrl Pts',(25.187903481163,65.1720018134176,206.193749999044));
#35719=CARTESIAN_POINT('Ctrl Pts',(25.798460424913,64.819496597588,206.135416665711));
#35720=CARTESIAN_POINT('Ctrl Pts',(26.409017368663,64.4669913817583,206.077083332377));
#35721=CARTESIAN_POINT('Ctrl Pts',(26.409017368663,63.761980950099,206.018749999044));
#35722=CARTESIAN_POINT('Ctrl Pts',(26.409017368663,63.0569705184397,205.960416665711));
#35723=CARTESIAN_POINT('Ctrl Pts',(25.798460424913,62.70446530261,205.902083332377));
#35724=CARTESIAN_POINT('Ctrl Pts',(25.187903481163,62.3519600867804,205.843749999044));
#35725=CARTESIAN_POINT('Ctrl Pts',(24.577346537413,62.70446530261,205.785416665711));
#35726=CARTESIAN_POINT('Ctrl Pts',(23.966789593663,63.0569705184397,205.727083332377));
#35727=CARTESIAN_POINT('Ctrl Pts',(23.966789593663,63.761980950099,205.668749999044));
#35728=CARTESIAN_POINT('Ctrl Pts',(23.966789593663,64.4669913817583,205.610416665711));
#35729=CARTESIAN_POINT('Ctrl Pts',(24.577346537413,64.819496597588,205.552083332377));
#35730=CARTESIAN_POINT('Ctrl Pts',(25.187903481163,65.1720018134176,205.493749999044));
#35731=CARTESIAN_POINT('Ctrl Pts',(25.798460424913,64.819496597588,205.435416665711));
#35732=CARTESIAN_POINT('Ctrl Pts',(26.409017368663,64.4669913817583,205.377083332377));
#35733=CARTESIAN_POINT('Ctrl Pts',(26.409017368663,63.761980950099,205.318749999044));
#35734=CARTESIAN_POINT('Ctrl Pts',(26.409017368663,63.0569705184397,205.260416665711));
#35735=CARTESIAN_POINT('Ctrl Pts',(25.798460424913,62.70446530261,205.202083332377));
#35736=CARTESIAN_POINT('Ctrl Pts',(25.187903481163,62.3519600867804,205.143749999044));
#35737=CARTESIAN_POINT('Ctrl Pts',(24.577346537413,62.70446530261,205.085416665711));
#35738=CARTESIAN_POINT('Ctrl Pts',(23.966789593663,63.0569705184397,205.027083332377));
#35739=CARTESIAN_POINT('Ctrl Pts',(23.966789593663,63.761980950099,204.968749999044));
#35740=CARTESIAN_POINT('Ctrl Pts',(23.966789593663,64.4669913817583,204.910416665711));
#35741=CARTESIAN_POINT('Ctrl Pts',(24.577346537413,64.819496597588,204.852083332377));
#35742=CARTESIAN_POINT('Ctrl Pts',(25.187903481163,65.1720018134176,204.793749999044));
#35743=CARTESIAN_POINT('Ctrl Pts',(25.798460424913,64.819496597588,204.735416665711));
#35744=CARTESIAN_POINT('Ctrl Pts',(26.409017368663,64.4669913817583,204.677083332377));
#35745=CARTESIAN_POINT('Ctrl Pts',(26.409017368663,63.761980950099,204.618749999044));
#35746=CARTESIAN_POINT('Ctrl Pts',(26.409017368663,63.0569705184397,204.560416665711));
#35747=CARTESIAN_POINT('Ctrl Pts',(25.798460424913,62.70446530261,204.502083332377));
#35748=CARTESIAN_POINT('Ctrl Pts',(25.187903481163,62.3519600867804,204.443749999044));
#35749=CARTESIAN_POINT('Ctrl Pts',(24.577346537413,62.70446530261,204.385416665711));
#35750=CARTESIAN_POINT('Ctrl Pts',(23.966789593663,63.0569705184397,204.327083332377));
#35751=CARTESIAN_POINT('Ctrl Pts',(23.966789593663,63.761980950099,204.268749999044));
#35752=CARTESIAN_POINT('Ctrl Pts',(23.966789593663,64.4669913817583,204.210416665711));
#35753=CARTESIAN_POINT('Ctrl Pts',(24.577346537413,64.819496597588,204.152083332377));
#35754=CARTESIAN_POINT('Ctrl Pts',(25.187903481163,65.1720018134176,204.093749999044));
#35755=CARTESIAN_POINT('Ctrl Pts',(25.798460424913,64.819496597588,204.035416665711));
#35756=CARTESIAN_POINT('Ctrl Pts',(26.409017368663,64.4669913817583,203.977083332377));
#35757=CARTESIAN_POINT('Ctrl Pts',(26.409017368663,63.761980950099,203.918749999044));
#35758=CARTESIAN_POINT('Ctrl Pts',(26.409017368663,63.0569705184397,203.860416665711));
#35759=CARTESIAN_POINT('Ctrl Pts',(25.798460424913,62.70446530261,203.802083332377));
#35760=CARTESIAN_POINT('Ctrl Pts',(25.187903481163,62.3519600867804,203.743749999044));
#35761=CARTESIAN_POINT('Ctrl Pts',(24.577346537413,62.70446530261,203.685416665711));
#35762=CARTESIAN_POINT('Ctrl Pts',(23.966789593663,63.0569705184397,203.627083332377));
#35763=CARTESIAN_POINT('Ctrl Pts',(23.966789593663,63.761980950099,203.568749999044));
#35764=CARTESIAN_POINT('Ctrl Pts',(23.966789593663,64.4669913817583,203.510416665711));
#35765=CARTESIAN_POINT('Ctrl Pts',(24.577346537413,64.819496597588,203.452083332377));
#35766=CARTESIAN_POINT('Ctrl Pts',(25.187903481163,65.1720018134176,203.393749999044));
#35767=CARTESIAN_POINT('Ctrl Pts',(25.798460424913,64.819496597588,203.335416665711));
#35768=CARTESIAN_POINT('Ctrl Pts',(26.409017368663,64.4669913817583,203.277083332377));
#35769=CARTESIAN_POINT('Ctrl Pts',(26.409017368663,63.761980950099,203.218749999044));
#35770=CARTESIAN_POINT('Ctrl Pts',(26.409017368663,63.0569705184397,203.160416665711));
#35771=CARTESIAN_POINT('Ctrl Pts',(25.798460424913,62.70446530261,203.102083332377));
#35772=CARTESIAN_POINT('Ctrl Pts',(25.187903481163,62.3519600867804,203.043749999044));
#35773=CARTESIAN_POINT('Ctrl Pts',(24.577346537413,62.70446530261,202.985416665711));
#35774=CARTESIAN_POINT('Ctrl Pts',(23.966789593663,63.0569705184397,202.927083332377));
#35775=CARTESIAN_POINT('Ctrl Pts',(23.966789593663,63.761980950099,202.868749999044));
#35776=CARTESIAN_POINT('Ctrl Pts',(23.966789593663,64.4669913817583,202.810416665711));
#35777=CARTESIAN_POINT('Ctrl Pts',(24.577346537413,64.819496597588,202.752083332377));
#35778=CARTESIAN_POINT('Ctrl Pts',(25.187903481163,65.1720018134176,202.693749999044));
#35779=CARTESIAN_POINT('Ctrl Pts',(25.798460424913,64.819496597588,202.635416665711));
#35780=CARTESIAN_POINT('Ctrl Pts',(26.409017368663,64.4669913817583,202.577083332377));
#35781=CARTESIAN_POINT('Ctrl Pts',(26.409017368663,63.761980950099,202.518749999044));
#35782=CARTESIAN_POINT('Ctrl Pts',(26.787903481163,63.761980950099,212.1));
#35783=CARTESIAN_POINT('Ctrl Pts',(26.787903481163,62.8382205193956,212.041666666667));
#35784=CARTESIAN_POINT('Ctrl Pts',(25.987903481163,62.3763403040439,211.983333333333));
#35785=CARTESIAN_POINT('Ctrl Pts',(25.187903481163,61.9144600886922,211.925));
#35786=CARTESIAN_POINT('Ctrl Pts',(24.387903481163,62.3763403040439,211.866666666667));
#35787=CARTESIAN_POINT('Ctrl Pts',(23.587903481163,62.8382205193956,211.808333333333));
#35788=CARTESIAN_POINT('Ctrl Pts',(23.587903481163,63.761980950099,211.75));
#35789=CARTESIAN_POINT('Ctrl Pts',(23.587903481163,64.6857413808024,211.691666666667));
#35790=CARTESIAN_POINT('Ctrl Pts',(24.387903481163,65.1476215961541,211.633333333333));
#35791=CARTESIAN_POINT('Ctrl Pts',(25.187903481163,65.6095018115058,211.575));
#35792=CARTESIAN_POINT('Ctrl Pts',(25.987903481163,65.1476215961541,211.516666666667));
#35793=CARTESIAN_POINT('Ctrl Pts',(26.787903481163,64.6857413808024,211.458333333333));
#35794=CARTESIAN_POINT('Ctrl Pts',(26.787903481163,63.761980950099,211.4));
#35795=CARTESIAN_POINT('Ctrl Pts',(26.787903481163,62.8382205193956,211.341666666667));
#35796=CARTESIAN_POINT('Ctrl Pts',(25.987903481163,62.3763403040439,211.283333333333));
#35797=CARTESIAN_POINT('Ctrl Pts',(25.187903481163,61.9144600886922,211.225));
#35798=CARTESIAN_POINT('Ctrl Pts',(24.387903481163,62.3763403040439,211.166666666667));
#35799=CARTESIAN_POINT('Ctrl Pts',(23.587903481163,62.8382205193956,211.108333333333));
#35800=CARTESIAN_POINT('Ctrl Pts',(23.587903481163,63.761980950099,211.05));
#35801=CARTESIAN_POINT('Ctrl Pts',(23.587903481163,64.6857413808024,210.991666666667));
#35802=CARTESIAN_POINT('Ctrl Pts',(24.387903481163,65.1476215961541,210.933333333333));
#35803=CARTESIAN_POINT('Ctrl Pts',(25.187903481163,65.6095018115058,210.875));
#35804=CARTESIAN_POINT('Ctrl Pts',(25.987903481163,65.1476215961541,210.816666666667));
#35805=CARTESIAN_POINT('Ctrl Pts',(26.787903481163,64.6857413808024,210.758333333333));
#35806=CARTESIAN_POINT('Ctrl Pts',(26.787903481163,63.761980950099,210.7));
#35807=CARTESIAN_POINT('Ctrl Pts',(26.787903481163,62.8382205193956,210.641666666667));
#35808=CARTESIAN_POINT('Ctrl Pts',(25.987903481163,62.3763403040439,210.583333333333));
#35809=CARTESIAN_POINT('Ctrl Pts',(25.187903481163,61.9144600886922,210.525));
#35810=CARTESIAN_POINT('Ctrl Pts',(24.387903481163,62.3763403040439,210.466666666667));
#35811=CARTESIAN_POINT('Ctrl Pts',(23.587903481163,62.8382205193956,210.408333333333));
#35812=CARTESIAN_POINT('Ctrl Pts',(23.587903481163,63.761980950099,210.35));
#35813=CARTESIAN_POINT('Ctrl Pts',(23.587903481163,64.6857413808024,210.291666666667));
#35814=CARTESIAN_POINT('Ctrl Pts',(24.387903481163,65.1476215961541,210.233333333333));
#35815=CARTESIAN_POINT('Ctrl Pts',(25.187903481163,65.6095018115058,210.175));
#35816=CARTESIAN_POINT('Ctrl Pts',(25.987903481163,65.1476215961541,210.116666666667));
#35817=CARTESIAN_POINT('Ctrl Pts',(26.787903481163,64.6857413808024,210.058333333333));
#35818=CARTESIAN_POINT('Ctrl Pts',(26.787903481163,63.761980950099,210.));
#35819=CARTESIAN_POINT('Ctrl Pts',(26.787903481163,62.8382205193956,209.941666666667));
#35820=CARTESIAN_POINT('Ctrl Pts',(25.987903481163,62.3763403040439,209.883333333333));
#35821=CARTESIAN_POINT('Ctrl Pts',(25.187903481163,61.9144600886922,209.825));
#35822=CARTESIAN_POINT('Ctrl Pts',(24.387903481163,62.3763403040439,209.766666666667));
#35823=CARTESIAN_POINT('Ctrl Pts',(23.587903481163,62.8382205193956,209.708333333333));
#35824=CARTESIAN_POINT('Ctrl Pts',(23.587903481163,63.761980950099,209.65));
#35825=CARTESIAN_POINT('Ctrl Pts',(23.587903481163,64.6857413808024,209.591666666667));
#35826=CARTESIAN_POINT('Ctrl Pts',(24.387903481163,65.1476215961541,209.533333333333));
#35827=CARTESIAN_POINT('Ctrl Pts',(25.187903481163,65.6095018115058,209.475));
#35828=CARTESIAN_POINT('Ctrl Pts',(25.987903481163,65.1476215961541,209.416666666667));
#35829=CARTESIAN_POINT('Ctrl Pts',(26.787903481163,64.6857413808024,209.358333333333));
#35830=CARTESIAN_POINT('Ctrl Pts',(26.787903481163,63.761980950099,209.3));
#35831=CARTESIAN_POINT('Ctrl Pts',(26.787903481163,62.8382205193956,209.241666666667));
#35832=CARTESIAN_POINT('Ctrl Pts',(25.987903481163,62.3763403040439,209.183333333333));
#35833=CARTESIAN_POINT('Ctrl Pts',(25.187903481163,61.9144600886922,209.125));
#35834=CARTESIAN_POINT('Ctrl Pts',(24.387903481163,62.3763403040439,209.066666666667));
#35835=CARTESIAN_POINT('Ctrl Pts',(23.587903481163,62.8382205193956,209.008333333333));
#35836=CARTESIAN_POINT('Ctrl Pts',(23.587903481163,63.761980950099,208.95));
#35837=CARTESIAN_POINT('Ctrl Pts',(23.587903481163,64.6857413808024,208.891666666667));
#35838=CARTESIAN_POINT('Ctrl Pts',(24.387903481163,65.1476215961541,208.833333333333));
#35839=CARTESIAN_POINT('Ctrl Pts',(25.187903481163,65.6095018115058,208.775));
#35840=CARTESIAN_POINT('Ctrl Pts',(25.987903481163,65.1476215961541,208.716666666667));
#35841=CARTESIAN_POINT('Ctrl Pts',(26.787903481163,64.6857413808024,208.658333333333));
#35842=CARTESIAN_POINT('Ctrl Pts',(26.787903481163,63.761980950099,208.6));
#35843=CARTESIAN_POINT('Ctrl Pts',(26.787903481163,62.8382205193956,208.541666666667));
#35844=CARTESIAN_POINT('Ctrl Pts',(25.987903481163,62.3763403040439,208.483333333333));
#35845=CARTESIAN_POINT('Ctrl Pts',(25.187903481163,61.9144600886922,208.425));
#35846=CARTESIAN_POINT('Ctrl Pts',(24.387903481163,62.3763403040439,208.366666666667));
#35847=CARTESIAN_POINT('Ctrl Pts',(23.587903481163,62.8382205193956,208.308333333333));
#35848=CARTESIAN_POINT('Ctrl Pts',(23.587903481163,63.761980950099,208.25));
#35849=CARTESIAN_POINT('Ctrl Pts',(23.587903481163,64.6857413808024,208.191666666667));
#35850=CARTESIAN_POINT('Ctrl Pts',(24.387903481163,65.1476215961541,208.133333333333));
#35851=CARTESIAN_POINT('Ctrl Pts',(25.187903481163,65.6095018115058,208.075));
#35852=CARTESIAN_POINT('Ctrl Pts',(25.987903481163,65.1476215961541,208.016666666667));
#35853=CARTESIAN_POINT('Ctrl Pts',(26.787903481163,64.6857413808024,207.958333333333));
#35854=CARTESIAN_POINT('Ctrl Pts',(26.787903481163,63.761980950099,207.9));
#35855=CARTESIAN_POINT('Ctrl Pts',(26.787903481163,62.8382205193956,207.841666666667));
#35856=CARTESIAN_POINT('Ctrl Pts',(25.987903481163,62.3763403040439,207.783333333333));
#35857=CARTESIAN_POINT('Ctrl Pts',(25.187903481163,61.9144600886922,207.725));
#35858=CARTESIAN_POINT('Ctrl Pts',(24.387903481163,62.3763403040439,207.666666666667));
#35859=CARTESIAN_POINT('Ctrl Pts',(23.587903481163,62.8382205193956,207.608333333333));
#35860=CARTESIAN_POINT('Ctrl Pts',(23.587903481163,63.761980950099,207.55));
#35861=CARTESIAN_POINT('Ctrl Pts',(23.587903481163,64.6857413808024,207.491666666667));
#35862=CARTESIAN_POINT('Ctrl Pts',(24.387903481163,65.1476215961541,207.433333333333));
#35863=CARTESIAN_POINT('Ctrl Pts',(25.187903481163,65.6095018115058,207.375));
#35864=CARTESIAN_POINT('Ctrl Pts',(25.987903481163,65.1476215961541,207.316666666667));
#35865=CARTESIAN_POINT('Ctrl Pts',(26.787903481163,64.6857413808024,207.258333333333));
#35866=CARTESIAN_POINT('Ctrl Pts',(26.787903481163,63.761980950099,207.2));
#35867=CARTESIAN_POINT('Ctrl Pts',(26.787903481163,62.8382205193956,207.141666666667));
#35868=CARTESIAN_POINT('Ctrl Pts',(25.987903481163,62.3763403040439,207.083333333333));
#35869=CARTESIAN_POINT('Ctrl Pts',(25.187903481163,61.9144600886922,207.025));
#35870=CARTESIAN_POINT('Ctrl Pts',(24.387903481163,62.3763403040439,206.966666666667));
#35871=CARTESIAN_POINT('Ctrl Pts',(23.587903481163,62.8382205193956,206.908333333333));
#35872=CARTESIAN_POINT('Ctrl Pts',(23.587903481163,63.761980950099,206.85));
#35873=CARTESIAN_POINT('Ctrl Pts',(23.587903481163,64.6857413808024,206.791666666667));
#35874=CARTESIAN_POINT('Ctrl Pts',(24.387903481163,65.1476215961541,206.733333333333));
#35875=CARTESIAN_POINT('Ctrl Pts',(25.187903481163,65.6095018115058,206.675));
#35876=CARTESIAN_POINT('Ctrl Pts',(25.987903481163,65.1476215961541,206.616666666667));
#35877=CARTESIAN_POINT('Ctrl Pts',(26.787903481163,64.6857413808024,206.558333333333));
#35878=CARTESIAN_POINT('Ctrl Pts',(26.787903481163,63.761980950099,206.5));
#35879=CARTESIAN_POINT('Ctrl Pts',(26.787903481163,62.8382205193956,206.441666666667));
#35880=CARTESIAN_POINT('Ctrl Pts',(25.987903481163,62.3763403040439,206.383333333333));
#35881=CARTESIAN_POINT('Ctrl Pts',(25.187903481163,61.9144600886922,206.325));
#35882=CARTESIAN_POINT('Ctrl Pts',(24.387903481163,62.3763403040439,206.266666666667));
#35883=CARTESIAN_POINT('Ctrl Pts',(23.587903481163,62.8382205193956,206.208333333333));
#35884=CARTESIAN_POINT('Ctrl Pts',(23.587903481163,63.761980950099,206.15));
#35885=CARTESIAN_POINT('Ctrl Pts',(23.587903481163,64.6857413808024,206.091666666667));
#35886=CARTESIAN_POINT('Ctrl Pts',(24.387903481163,65.1476215961541,206.033333333333));
#35887=CARTESIAN_POINT('Ctrl Pts',(25.187903481163,65.6095018115058,205.975));
#35888=CARTESIAN_POINT('Ctrl Pts',(25.987903481163,65.1476215961541,205.916666666667));
#35889=CARTESIAN_POINT('Ctrl Pts',(26.787903481163,64.6857413808024,205.858333333333));
#35890=CARTESIAN_POINT('Ctrl Pts',(26.787903481163,63.761980950099,205.8));
#35891=CARTESIAN_POINT('Ctrl Pts',(26.787903481163,62.8382205193956,205.741666666667));
#35892=CARTESIAN_POINT('Ctrl Pts',(25.987903481163,62.3763403040439,205.683333333333));
#35893=CARTESIAN_POINT('Ctrl Pts',(25.187903481163,61.9144600886922,205.625));
#35894=CARTESIAN_POINT('Ctrl Pts',(24.387903481163,62.3763403040439,205.566666666667));
#35895=CARTESIAN_POINT('Ctrl Pts',(23.587903481163,62.8382205193956,205.508333333333));
#35896=CARTESIAN_POINT('Ctrl Pts',(23.587903481163,63.761980950099,205.45));
#35897=CARTESIAN_POINT('Ctrl Pts',(23.587903481163,64.6857413808024,205.391666666667));
#35898=CARTESIAN_POINT('Ctrl Pts',(24.387903481163,65.1476215961541,205.333333333333));
#35899=CARTESIAN_POINT('Ctrl Pts',(25.187903481163,65.6095018115058,205.275));
#35900=CARTESIAN_POINT('Ctrl Pts',(25.987903481163,65.1476215961541,205.216666666667));
#35901=CARTESIAN_POINT('Ctrl Pts',(26.787903481163,64.6857413808024,205.158333333333));
#35902=CARTESIAN_POINT('Ctrl Pts',(26.787903481163,63.761980950099,205.1));
#35903=CARTESIAN_POINT('Ctrl Pts',(26.787903481163,62.8382205193956,205.041666666667));
#35904=CARTESIAN_POINT('Ctrl Pts',(25.987903481163,62.3763403040439,204.983333333333));
#35905=CARTESIAN_POINT('Ctrl Pts',(25.187903481163,61.9144600886922,204.925));
#35906=CARTESIAN_POINT('Ctrl Pts',(24.387903481163,62.3763403040439,204.866666666667));
#35907=CARTESIAN_POINT('Ctrl Pts',(23.587903481163,62.8382205193956,204.808333333333));
#35908=CARTESIAN_POINT('Ctrl Pts',(23.587903481163,63.761980950099,204.75));
#35909=CARTESIAN_POINT('Ctrl Pts',(23.587903481163,64.6857413808024,204.691666666667));
#35910=CARTESIAN_POINT('Ctrl Pts',(24.387903481163,65.1476215961541,204.633333333333));
#35911=CARTESIAN_POINT('Ctrl Pts',(25.187903481163,65.6095018115058,204.575));
#35912=CARTESIAN_POINT('Ctrl Pts',(25.987903481163,65.1476215961541,204.516666666667));
#35913=CARTESIAN_POINT('Ctrl Pts',(26.787903481163,64.6857413808024,204.458333333333));
#35914=CARTESIAN_POINT('Ctrl Pts',(26.787903481163,63.761980950099,204.4));
#35915=CARTESIAN_POINT('Ctrl Pts',(26.787903481163,62.8382205193956,204.341666666667));
#35916=CARTESIAN_POINT('Ctrl Pts',(25.987903481163,62.3763403040439,204.283333333333));
#35917=CARTESIAN_POINT('Ctrl Pts',(25.187903481163,61.9144600886922,204.225));
#35918=CARTESIAN_POINT('Ctrl Pts',(24.387903481163,62.3763403040439,204.166666666667));
#35919=CARTESIAN_POINT('Ctrl Pts',(23.587903481163,62.8382205193956,204.108333333333));
#35920=CARTESIAN_POINT('Ctrl Pts',(23.587903481163,63.761980950099,204.05));
#35921=CARTESIAN_POINT('Ctrl Pts',(23.587903481163,64.6857413808024,203.991666666667));
#35922=CARTESIAN_POINT('Ctrl Pts',(24.387903481163,65.1476215961541,203.933333333333));
#35923=CARTESIAN_POINT('Ctrl Pts',(25.187903481163,65.6095018115058,203.875));
#35924=CARTESIAN_POINT('Ctrl Pts',(25.987903481163,65.1476215961541,203.816666666667));
#35925=CARTESIAN_POINT('Ctrl Pts',(26.787903481163,64.6857413808024,203.758333333333));
#35926=CARTESIAN_POINT('Ctrl Pts',(26.787903481163,63.761980950099,203.7));
#35927=CARTESIAN_POINT('Ctrl Pts',(26.787903481163,62.8382205193956,203.641666666667));
#35928=CARTESIAN_POINT('Ctrl Pts',(25.987903481163,62.3763403040439,203.583333333333));
#35929=CARTESIAN_POINT('Ctrl Pts',(25.187903481163,61.9144600886922,203.525));
#35930=CARTESIAN_POINT('Ctrl Pts',(24.387903481163,62.3763403040439,203.466666666667));
#35931=CARTESIAN_POINT('Ctrl Pts',(23.587903481163,62.8382205193956,203.408333333333));
#35932=CARTESIAN_POINT('Ctrl Pts',(23.587903481163,63.761980950099,203.35));
#35933=CARTESIAN_POINT('Ctrl Pts',(23.587903481163,64.6857413808024,203.291666666667));
#35934=CARTESIAN_POINT('Ctrl Pts',(24.387903481163,65.1476215961541,203.233333333333));
#35935=CARTESIAN_POINT('Ctrl Pts',(25.187903481163,65.6095018115058,203.175));
#35936=CARTESIAN_POINT('Ctrl Pts',(25.987903481163,65.1476215961541,203.116666666667));
#35937=CARTESIAN_POINT('Ctrl Pts',(26.787903481163,64.6857413808024,203.058333333333));
#35938=CARTESIAN_POINT('Ctrl Pts',(26.787903481163,63.761980950099,203.));
#35939=CARTESIAN_POINT('Ctrl Pts',(26.787903481163,62.8382205193956,202.941666666667));
#35940=CARTESIAN_POINT('Ctrl Pts',(25.987903481163,62.3763403040439,202.883333333333));
#35941=CARTESIAN_POINT('Ctrl Pts',(25.187903481163,61.9144600886922,202.825));
#35942=CARTESIAN_POINT('Ctrl Pts',(24.387903481163,62.3763403040439,202.766666666667));
#35943=CARTESIAN_POINT('Ctrl Pts',(23.587903481163,62.8382205193956,202.708333333333));
#35944=CARTESIAN_POINT('Ctrl Pts',(23.587903481163,63.761980950099,202.65));
#35945=CARTESIAN_POINT('Ctrl Pts',(23.587903481163,64.6857413808024,202.591666666667));
#35946=CARTESIAN_POINT('Ctrl Pts',(24.387903481163,65.1476215961541,202.533333333333));
#35947=CARTESIAN_POINT('Ctrl Pts',(25.187903481163,65.6095018115058,202.475));
#35948=CARTESIAN_POINT('Ctrl Pts',(25.987903481163,65.1476215961541,202.416666666667));
#35949=CARTESIAN_POINT('Ctrl Pts',(26.787903481163,64.6857413808024,202.358333333333));
#35950=CARTESIAN_POINT('Ctrl Pts',(26.787903481163,63.761980950099,202.3));
#35951=CARTESIAN_POINT('',(26.598460424913,63.761980950099,212.209374999522));
#35952=CARTESIAN_POINT('Ctrl Pts',(26.787903481163,63.761980950099,212.1));
#35953=CARTESIAN_POINT('Ctrl Pts',(26.787903481163,63.5528822225132,212.086795899272));
#35954=CARTESIAN_POINT('Ctrl Pts',(26.7469152133774,63.3458641356268,212.072228822259));
#35955=CARTESIAN_POINT('Ctrl Pts',(26.5867614174791,62.957027061243,212.041835720424));
#35956=CARTESIAN_POINT('Ctrl Pts',(26.4681877346425,62.7793122371604,212.026290441717));
#35957=CARTESIAN_POINT('Ctrl Pts',(26.1715229442533,62.4830672025603,211.996767349568));
#35958=CARTESIAN_POINT('Ctrl Pts',(25.9974726268862,62.3663763860522,211.984031083542));
#35959=CARTESIAN_POINT('Ctrl Pts',(25.6158431081187,62.2065561348171,211.956203931132));
#35960=CARTESIAN_POINT('Ctrl Pts',(25.412171684918,62.1644358549729,211.941352889857));
#35961=CARTESIAN_POINT('Ctrl Pts',(24.9920026023566,62.159641416223,211.91071556092));
#35962=CARTESIAN_POINT('Ctrl Pts',(24.7794798571627,62.2002214897408,211.89521911075));
#35963=CARTESIAN_POINT('Ctrl Pts',(24.3930591021861,62.358565076682,211.867042597366));
#35964=CARTESIAN_POINT('Ctrl Pts',(24.2213486307701,62.4708047689436,211.854629142074));
#35965=CARTESIAN_POINT('Ctrl Pts',(23.9253596763751,62.7572595686795,211.825748920453));
#35966=CARTESIAN_POINT('Ctrl Pts',(23.8053148587378,62.9301656277874,211.810453669002));
#35967=CARTESIAN_POINT('Ctrl Pts',(23.6368471212299,63.3156176230095,211.779971214628));
#35968=CARTESIAN_POINT('Ctrl Pts',(23.5913649953638,63.5250588476194,211.7650872835));
#35969=CARTESIAN_POINT('Ctrl Pts',(23.5849639057201,63.9403798129072,211.738627352662));
#35970=CARTESIAN_POINT('Ctrl Pts',(23.6205201181075,64.1423015128207,211.724794488421));
#35971=CARTESIAN_POINT('Ctrl Pts',(23.7681882652492,64.5293978139233,211.694966518335));
#35972=CARTESIAN_POINT('Ctrl Pts',(23.8816542499166,64.7097359091757,211.679441804286));
#35973=CARTESIAN_POINT('Ctrl Pts',(24.1707256249538,65.0146100844818,211.64965064514));
#35974=CARTESIAN_POINT('Ctrl Pts',(24.3429020179363,65.1366372748414,211.636614690027));
#35975=CARTESIAN_POINT('Ctrl Pts',(24.7213214416994,65.3061875351901,211.609021607044));
#35976=CARTESIAN_POINT('Ctrl Pts',(24.9233666896425,65.3532878029956,211.594289141048));
#35977=CARTESIAN_POINT('Ctrl Pts',(25.3422082252478,65.3687851666763,211.56374861241));
#35978=CARTESIAN_POINT('Ctrl Pts',(25.5551431832926,65.3338567177254,211.548222105053));
#35979=CARTESIAN_POINT('Ctrl Pts',(25.9456448926417,65.1858542596342,211.51974802208));
#35980=CARTESIAN_POINT('Ctrl Pts',(26.1207180230927,65.0778263003631,211.507417058424));
#35981=CARTESIAN_POINT('Ctrl Pts',(26.4239592468199,64.7990100221814,211.478754786108));
#35982=CARTESIAN_POINT('Ctrl Pts',(26.5481450116235,64.6297298167745,211.463537526895));
#35983=CARTESIAN_POINT('Ctrl Pts',(26.726580176644,64.249330335995,211.43301073132));
#35984=CARTESIAN_POINT('Ctrl Pts',(26.7776079136368,64.0411270257476,211.41800278788));
#35985=CARTESIAN_POINT('Ctrl Pts',(26.7874362346422,63.8066458051222,211.402837517256));
#35986=CARTESIAN_POINT('Ctrl Pts',(26.787903481163,63.7843058451588,211.401409765456));
#35987=CARTESIAN_POINT('Ctrl Pts',(26.787903481163,63.7619809500992,211.4));
#35988=CARTESIAN_POINT('',(26.787903481163,63.761980950099,202.3));
#35989=CARTESIAN_POINT('Ctrl Pts',(23.7486592957405,64.4609631921677,202.6));
#35990=CARTESIAN_POINT('Ctrl Pts',(23.9630003818437,64.9023036773826,202.564315850992));
#35991=CARTESIAN_POINT('Ctrl Pts',(24.387903481163,65.1476215961541,202.533333333333));
#35992=CARTESIAN_POINT('Ctrl Pts',(25.187903481163,65.6095018115058,202.475));
#35993=CARTESIAN_POINT('Ctrl Pts',(25.987903481163,65.1476215961541,202.416666666667));
#35994=CARTESIAN_POINT('Ctrl Pts',(26.787903481163,64.6857413808024,202.358333333333));
#35995=CARTESIAN_POINT('Ctrl Pts',(26.787903481163,63.761980950099,202.3));
#35996=CARTESIAN_POINT('',(26.598460424913,63.761980950099,202.409374999522));
#35997=CARTESIAN_POINT('Origin',(26.598460424913,63.761980950099,202.409374999522));
#35998=CARTESIAN_POINT('',(26.787903481163,63.761980950099,202.606249999044));
#35999=CARTESIAN_POINT('Origin',(26.598460424913,63.761980950099,212.209374999522));
#36000=CARTESIAN_POINT('Origin',(25.1879034811632,63.761980950099,212.406249999044));
#36001=CARTESIAN_POINT('Origin',(25.187903481163,63.761980950099,202.6));
#36002=CARTESIAN_POINT('Origin',(25.187903481163,63.761980950099,212.1));
#36003=CARTESIAN_POINT('',(23.187903481163,63.761980950099,212.5));
#36004=CARTESIAN_POINT('',(23.587903481163,63.761980950099,212.1));
#36005=CARTESIAN_POINT('Origin',(25.187903481163,63.761980950099,212.5));
#36006=CARTESIAN_POINT('Origin',(25.187903481163,63.761980950099,202.2));
#36007=CARTESIAN_POINT('',(27.187903481163,63.761980950099,202.2));
#36008=CARTESIAN_POINT('Origin',(25.187903481163,63.761980950099,212.5));
#36009=CARTESIAN_POINT('',(21.2239277116833,64.2976077782208,212.1));
#36010=CARTESIAN_POINT('',(29.187903481163,63.761980950099,212.1));
#36011=CARTESIAN_POINT('Origin',(25.187903481163,63.761980950099,212.1));
#36012=CARTESIAN_POINT('Origin',(25.187903481163,63.761980950099,212.1));
#36013=CARTESIAN_POINT('',(28.787903481163,63.761980950099,212.5));
#36014=CARTESIAN_POINT('',(28.787903481163,63.761980950099,212.5));
#36015=CARTESIAN_POINT('Origin',(25.187903481163,63.761980950099,212.5));
#36016=CARTESIAN_POINT('Origin',(25.187903481163,63.761980950099,212.5));
#36017=CARTESIAN_POINT('Origin',(25.187903481163,63.761980950099,212.5));
#36018=CARTESIAN_POINT('Origin',(19.9513700273636,43.5818784659284,205.8));
#36019=CARTESIAN_POINT('Origin',(-18.1629964860985,83.0516975441391,209.8));
#36020=CARTESIAN_POINT('',(-13.2080267742527,82.3821640089894,209.8));
#36021=CARTESIAN_POINT('Origin',(-18.1629964860985,83.0516975441391,209.8));
#36022=CARTESIAN_POINT('',(-13.7035237454372,82.4491173625044,210.3));
#36023=CARTESIAN_POINT('Origin',(-13.7035237454372,82.4491173625044,209.8));
#36024=CARTESIAN_POINT('Origin',(-18.1629964860985,83.0516975441391,210.3));
#36025=CARTESIAN_POINT('Origin',(-18.1629964860985,83.0516975441391,201.8));
#36026=CARTESIAN_POINT('',(-13.7035237454372,82.4491173625044,201.3));
#36027=CARTESIAN_POINT('Origin',(-18.1629964860985,83.0516975441391,201.3));
#36028=CARTESIAN_POINT('',(-13.2080267742527,82.3821640089894,201.8));
#36029=CARTESIAN_POINT('Origin',(-13.7035237454372,82.4491173625044,201.8));
#36030=CARTESIAN_POINT('Origin',(-18.1629964860985,83.0516975441391,201.8));
#36031=CARTESIAN_POINT('Origin',(-18.1629964860985,83.0516975441391,210.3));
#36032=CARTESIAN_POINT('',(-13.2080267742527,82.3821640089894,210.3));
#36033=CARTESIAN_POINT('Origin',(25.18790348116,63.761980950101,201.3));
#36034=CARTESIAN_POINT('',(18.2509458845758,64.6993278993105,211.3));
#36035=CARTESIAN_POINT('Origin',(25.18790348116,63.761980950101,211.3));
#36036=CARTESIAN_POINT('',(18.2509458845758,64.6993278993105,201.3));
#36037=CARTESIAN_POINT('Origin',(43.0811453810906,77.1117683798125,211.3));
#36038=CARTESIAN_POINT('',(40.5678791273553,80.5028251540171,209.3));
#36039=CARTESIAN_POINT('',(45.6182378895769,73.7385006893635,209.3));
#36040=CARTESIAN_POINT('Origin',(43.0811453810902,77.1117683798122,209.3));
#36041=CARTESIAN_POINT('',(40.5678791273553,80.5028251540171,210.3));
#36042=CARTESIAN_POINT('',(40.5678791273553,80.5028251540171,211.3));
#36043=CARTESIAN_POINT('',(45.6182378895769,73.7385006893635,210.3));
#36044=CARTESIAN_POINT('Origin',(43.0811453810904,77.1117683798123,210.3));
#36045=CARTESIAN_POINT('',(45.6182378895769,73.7385006893635,211.3));
#36046=CARTESIAN_POINT('Origin',(-18.1629964860985,83.0516975441391,214.3));
#36047=CARTESIAN_POINT('',(-16.5774061783079,82.8374468128912,210.3));
#36048=CARTESIAN_POINT('Origin',(-18.1629964860985,83.0516975441391,210.3));
#36049=CARTESIAN_POINT('',(-16.5774061783079,82.8374468128912,211.3));
#36050=CARTESIAN_POINT('',(-16.5774061783079,82.8374468128912,214.3));
#36051=CARTESIAN_POINT('Origin',(-18.1629964860985,83.0516975441391,211.3));
#36052=CARTESIAN_POINT('Origin',(19.9513700273636,43.5818784659284,211.3));
#36053=CARTESIAN_POINT('',(33.0886175986719,60.6545323126593,211.3));
#36054=CARTESIAN_POINT('',(27.3961507532244,48.8565674904361,211.3));
#36055=CARTESIAN_POINT('',(33.0886175986719,60.6545323126593,211.3));
#36056=CARTESIAN_POINT('',(16.5874683335563,50.6796992602564,211.3));
#36057=CARTESIAN_POINT('',(16.5874683335563,50.6796992602564,211.3));
#36058=CARTESIAN_POINT('',(17.9737067090166,58.898200306828,211.3));
#36059=CARTESIAN_POINT('',(17.9737067090166,58.898200306828,211.3));
#36060=CARTESIAN_POINT('',(17.1520153223208,60.475703333365,211.3));
#36061=CARTESIAN_POINT('',(17.9737067090166,58.898200306828,211.3));
#36062=CARTESIAN_POINT('',(15.7499363351254,62.4777857800405,211.3));
#36063=CARTESIAN_POINT('',(17.1520153223208,60.475703333365,211.3));
#36064=CARTESIAN_POINT('',(-15.5987525505707,76.8301353719087,211.3));
#36065=CARTESIAN_POINT('',(15.7499363351254,62.4777857800405,211.3));
#36066=CARTESIAN_POINT('',(-20.5710649571149,78.5071727628224,211.3));
#36067=CARTESIAN_POINT('',(-15.5987525505707,76.8301353719087,211.3));
#36068=CARTESIAN_POINT('',(-14.5190710707069,86.6812025814917,211.3));
#36069=CARTESIAN_POINT('Origin',(-18.1629964860985,83.0516975441391,211.3));
#36070=CARTESIAN_POINT('',(-11.7413224523512,83.8924176965482,211.3));
#36071=CARTESIAN_POINT('',(-14.5190710707069,86.6812025814917,211.3));
#36072=CARTESIAN_POINT('',(8.52323991612264,75.4822066097016,211.3));
#36073=CARTESIAN_POINT('',(-11.7413224523512,83.8924176965482,211.3));
#36074=CARTESIAN_POINT('',(26.4178380401533,73.0642234051985,211.3));
#36075=CARTESIAN_POINT('',(8.52323991612264,75.4822066097016,211.3));
#36076=CARTESIAN_POINT('',(30.5560117383973,75.2396394283021,211.3));
#36077=CARTESIAN_POINT('',(26.4178380401533,73.0642234051985,211.3));
#36078=CARTESIAN_POINT('',(38.4831850337045,66.2877716357375,211.3));
#36079=CARTESIAN_POINT('',(41.6077496400986,62.7593147414841,211.3));
#36080=CARTESIAN_POINT('',(45.6182378895769,73.7385006893635,211.3));
#36081=CARTESIAN_POINT('Origin',(19.9513700273636,43.5818784659284,211.3));
#36082=CARTESIAN_POINT('',(23.5430846542788,40.8708664706021,212.8));
#36083=CARTESIAN_POINT('',(15.4918972867023,44.1844586475632,212.8));
#36084=CARTESIAN_POINT('Origin',(19.9513700273636,43.5818784659284,212.8));
#36085=CARTESIAN_POINT('',(23.5430846542788,40.8708664706021,213.8));
#36086=CARTESIAN_POINT('',(23.5430846542788,40.8708664706021,211.3));
#36087=CARTESIAN_POINT('',(15.4918972867023,44.1844586475632,213.8));
#36088=CARTESIAN_POINT('Origin',(19.9513700273636,43.5818784659284,213.8));
#36089=CARTESIAN_POINT('',(15.4918972867023,44.1844586475632,211.3));
#36090=CARTESIAN_POINT('Origin',(19.9513700273636,43.5818784659284,212.3));
#36091=CARTESIAN_POINT('',(16.8325960933951,52.1329722228591,212.3));
#36092=CARTESIAN_POINT('',(17.9737067090166,58.898200306828,212.3));
#36093=CARTESIAN_POINT('',(17.9737067090166,58.898200306828,212.3));
#36094=CARTESIAN_POINT('',(28.0630252423339,50.2387032106721,212.3));
#36095=CARTESIAN_POINT('',(27.8913277021599,50.2676639320753,212.3));
#36096=CARTESIAN_POINT('',(33.0886175986719,60.6545323126593,212.3));
#36097=CARTESIAN_POINT('',(33.0886175986719,60.6545323126593,212.3));
#36098=CARTESIAN_POINT('',(39.0756626604441,66.9064622546218,212.3));
#36099=CARTESIAN_POINT('',(45.6182378895769,73.7385006893635,212.3));
#36100=CARTESIAN_POINT('',(31.6613562950968,75.8207132147201,212.3));
#36101=CARTESIAN_POINT('',(42.7226967777198,62.5216181735379,212.3));
#36102=CARTESIAN_POINT('',(26.4178380401533,73.0642234051985,212.3));
#36103=CARTESIAN_POINT('',(26.4178380401533,73.0642234051985,212.3));
#36104=CARTESIAN_POINT('',(8.52323991612264,75.4822066097016,212.3));
#36105=CARTESIAN_POINT('',(8.52323991612264,75.4822066097016,212.3));
#36106=CARTESIAN_POINT('',(-11.7413224523512,83.8924176965482,212.3));
#36107=CARTESIAN_POINT('',(-11.7413224523512,83.8924176965482,212.3));
#36108=CARTESIAN_POINT('',(-14.5190710707069,86.6812025814917,212.3));
#36109=CARTESIAN_POINT('',(-14.5190710707069,86.6812025814917,212.3));
#36110=CARTESIAN_POINT('',(-20.5710649571149,78.5071727628224,212.3));
#36111=CARTESIAN_POINT('Origin',(-18.1629964860985,83.0516975441391,212.3));
#36112=CARTESIAN_POINT('',(-15.5987525505707,76.8301353719087,212.3));
#36113=CARTESIAN_POINT('',(-15.5987525505707,76.8301353719087,212.3));
#36114=CARTESIAN_POINT('',(15.7499363351254,62.4777857800405,212.3));
#36115=CARTESIAN_POINT('',(15.7499363351254,62.4777857800405,212.3));
#36116=CARTESIAN_POINT('',(17.1520153223208,60.475703333365,212.3));
#36117=CARTESIAN_POINT('',(17.1520153223208,60.475703333365,212.3));
#36118=CARTESIAN_POINT('',(17.9737067090166,58.898200306828,212.3));
#36119=CARTESIAN_POINT('',(21.2239277116833,64.2976077782208,212.3));
#36120=CARTESIAN_POINT('Origin',(25.18790348116,63.761980950101,212.3));
#36121=CARTESIAN_POINT('',(-15.7623923893876,80.4345282249253,212.3));
#36122=CARTESIAN_POINT('',(-14.7228500730009,83.7738348943986,212.3));
#36123=CARTESIAN_POINT('',(-15.7623923893876,80.4345282249253,212.3));
#36124=CARTESIAN_POINT('',(-19.1740879543717,79.6651449444885,212.3));
#36125=CARTESIAN_POINT('',(-19.1740879543717,79.6651449444885,212.3));
#36126=CARTESIAN_POINT('',(-21.546241202969,82.235068333525,212.3));
#36127=CARTESIAN_POINT('',(-21.546241202969,82.235068333525,212.3));
#36128=CARTESIAN_POINT('',(-20.5066988865823,85.5743750029983,212.3));
#36129=CARTESIAN_POINT('',(-20.5066988865823,85.5743750029983,212.3));
#36130=CARTESIAN_POINT('',(-17.0950033215982,86.3437582834351,212.3));
#36131=CARTESIAN_POINT('',(-17.0950033215982,86.3437582834351,212.3));
#36132=CARTESIAN_POINT('',(-14.7228500730009,83.7738348943986,212.3));
#36133=CARTESIAN_POINT('Origin',(17.9737067090166,58.898200306828,211.3));
#36134=CARTESIAN_POINT('',(16.6330079023238,50.9496867315321,213.8));
#36135=CARTESIAN_POINT('',(15.4918972867023,44.1844586475632,213.8));
#36136=CARTESIAN_POINT('',(16.7328019978594,51.5413294771956,213.2));
#36137=CARTESIAN_POINT('Origin',(16.6330079023238,50.9496867315321,213.2));
#36138=CARTESIAN_POINT('',(16.7328019978594,51.5413294771956,212.9));
#36139=CARTESIAN_POINT('',(16.7328019978594,51.5413294771956,213.8));
#36140=CARTESIAN_POINT('Origin',(16.8325960933951,52.1329722228591,212.9));
#36141=CARTESIAN_POINT('',(17.9737067090166,58.898200306828,211.3));
#36142=CARTESIAN_POINT('',(16.4876742380207,50.088056514593,211.9));
#36143=CARTESIAN_POINT('Origin',(16.5874683335563,50.6796992602564,211.9));
#36144=CARTESIAN_POINT('',(16.4876742380207,50.088056514593,212.2));
#36145=CARTESIAN_POINT('',(16.4876742380207,50.088056514593,212.8));
#36146=CARTESIAN_POINT('',(16.387880142485,49.4964137689295,212.8));
#36147=CARTESIAN_POINT('Origin',(16.387880142485,49.4964137689295,212.2));
#36148=CARTESIAN_POINT('',(16.4876742380207,50.088056514593,212.8));
#36149=CARTESIAN_POINT('Origin',(17.9737067090166,58.898200306828,211.3));
#36150=CARTESIAN_POINT('',(17.1520153223208,60.475703333365,211.3));
#36151=CARTESIAN_POINT('Origin',(17.1520153223208,60.475703333365,211.3));
#36152=CARTESIAN_POINT('',(15.7499363351254,62.4777857800405,211.3));
#36153=CARTESIAN_POINT('Origin',(15.7499363351254,62.4777857800405,211.3));
#36154=CARTESIAN_POINT('',(-15.5987525505707,76.8301353719087,211.3));
#36155=CARTESIAN_POINT('Origin',(-15.5987525505707,76.8301353719087,211.3));
#36156=CARTESIAN_POINT('',(-20.5710649571149,78.5071727628224,211.3));
#36157=CARTESIAN_POINT('Origin',(-18.1629964860985,83.0516975441391,211.3));
#36158=CARTESIAN_POINT('',(-14.5190710707069,86.6812025814917,211.3));
#36159=CARTESIAN_POINT('Origin',(-14.5190710707069,86.6812025814917,211.3));
#36160=CARTESIAN_POINT('',(-11.7413224523512,83.8924176965482,211.3));
#36161=CARTESIAN_POINT('Origin',(-11.7413224523512,83.8924176965482,211.3));
#36162=CARTESIAN_POINT('',(8.52323991612264,75.4822066097016,211.3));
#36163=CARTESIAN_POINT('Origin',(8.52323991612264,75.4822066097016,211.3));
#36164=CARTESIAN_POINT('',(26.4178380401533,73.0642234051985,211.3));
#36165=CARTESIAN_POINT('Origin',(26.4178380401533,73.0642234051985,211.3));
#36166=CARTESIAN_POINT('',(32.2948489085972,76.1537369305954,211.6));
#36167=CARTESIAN_POINT('Origin',(31.6613562950993,75.8207132147214,211.600000000003));
#36168=CARTESIAN_POINT('',(32.2948489085972,76.1537369305954,211.));
#36169=CARTESIAN_POINT('',(32.2948489085972,76.1537369305954,210.3));
#36170=CARTESIAN_POINT('',(32.9283415220976,76.4867606464707,210.3));
#36171=CARTESIAN_POINT('Origin',(32.9283415220973,76.4867606464705,211.));
#36172=CARTESIAN_POINT('',(32.2948489085972,76.1537369305954,210.3));
#36173=CARTESIAN_POINT('',(31.8320221920213,75.9104313739469,209.3));
#36174=CARTESIAN_POINT('',(31.1940169652093,75.5750354011245,209.3));
#36175=CARTESIAN_POINT('',(31.1940169652093,75.5750354011245,210.));
#36176=CARTESIAN_POINT('Origin',(31.8320221920246,75.9104313739487,210.000000000003));
#36177=CARTESIAN_POINT('',(31.1940169652093,75.5750354011245,210.6));
#36178=CARTESIAN_POINT('',(31.1940169652093,75.5750354011245,209.3));
#36179=CARTESIAN_POINT('Origin',(30.5560117383975,75.2396394283022,210.6));
#36180=CARTESIAN_POINT('Origin',(45.6182378895769,73.7385006893635,211.3));
#36181=CARTESIAN_POINT('',(39.56293242615,67.4152903002768,211.));
#36182=CARTESIAN_POINT('',(39.56293242615,67.4152903002768,211.6));
#36183=CARTESIAN_POINT('',(39.56293242615,67.4152903002768,210.3));
#36184=CARTESIAN_POINT('Origin',(39.0756626604456,66.9064622546234,211.600000000002));
#36185=CARTESIAN_POINT('',(33.0886175986719,60.6545323126593,211.3));
#36186=CARTESIAN_POINT('',(38.9689769974974,66.7950564970781,210.6));
#36187=CARTESIAN_POINT('Origin',(38.4831850337063,66.2877716357394,210.600000000002));
#36188=CARTESIAN_POINT('',(38.9689769974974,66.7950564970781,210.));
#36189=CARTESIAN_POINT('',(38.9689769974974,66.7950564970781,209.3));
#36190=CARTESIAN_POINT('',(39.4547689612902,67.3023413584188,209.3));
#36191=CARTESIAN_POINT('Origin',(39.454768961292,67.3023413584207,210.000000000003));
#36192=CARTESIAN_POINT('',(45.6182378895769,73.7385006893635,209.3));
#36193=CARTESIAN_POINT('',(40.0502021918559,67.9241183459317,210.3));
#36194=CARTESIAN_POINT('',(39.56293242615,67.4152903002768,210.3));
#36195=CARTESIAN_POINT('Origin',(40.0502021918592,67.9241183459352,211.000000000005));
#36196=CARTESIAN_POINT('Origin',(33.0886175986719,60.6545323126593,211.3));
#36197=CARTESIAN_POINT('',(27.7915336066242,49.6760211864118,213.2));
#36198=CARTESIAN_POINT('',(27.7915336066242,49.6760211864118,212.9));
#36199=CARTESIAN_POINT('',(27.7915336066242,49.6760211864118,213.8));
#36200=CARTESIAN_POINT('',(27.5200419709145,49.1133391621515,213.8));
#36201=CARTESIAN_POINT('Origin',(27.5200419709149,49.1133391621524,213.200000000001));
#36202=CARTESIAN_POINT('',(27.7915336066242,49.6760211864118,213.8));
#36203=CARTESIAN_POINT('',(26.853167481805,47.7312034419155,212.8));
#36204=CARTESIAN_POINT('',(23.5430846542788,40.8708664706021,212.8));
#36205=CARTESIAN_POINT('',(27.1246591175147,48.2938854661758,212.2));
#36206=CARTESIAN_POINT('Origin',(26.8531674818047,47.7312034419149,212.199999999999));
#36207=CARTESIAN_POINT('',(27.1246591175147,48.2938854661758,211.9));
#36208=CARTESIAN_POINT('',(27.1246591175147,48.2938854661758,212.8));
#36209=CARTESIAN_POINT('Origin',(27.3961507532234,48.856567490434,211.899999999998));
#36210=CARTESIAN_POINT('Origin',(28.0630252423357,50.2387032106758,212.900000000004));
#36211=CARTESIAN_POINT('Origin',(43.0811453810902,77.1117683798122,209.3));
#36212=CARTESIAN_POINT('',(31.7180758735483,76.03910679713,209.3));
#36213=CARTESIAN_POINT('Origin',(38.9689769974974,66.7950564970781,209.3));
#36214=CARTESIAN_POINT('',(38.9689769974974,66.7950564970781,210.6));
#36215=CARTESIAN_POINT('',(38.9689769974974,66.7950564970781,210.));
#36216=CARTESIAN_POINT('Origin',(32.2948489085972,76.1537369305954,210.3));
#36217=CARTESIAN_POINT('',(32.2948489085972,76.1537369305954,211.));
#36218=CARTESIAN_POINT('',(32.2948489085972,76.1537369305954,211.6));
#36219=CARTESIAN_POINT('Origin',(43.0811453810904,77.1117683798123,210.3));
#36220=CARTESIAN_POINT('',(40.1011097736976,67.8629119514361,210.3));
#36221=CARTESIAN_POINT('Origin',(36.7726348574482,71.8647509982436,211.));
#36222=CARTESIAN_POINT('Origin',(31.7566715610496,75.7061152794361,211.6));
#36223=CARTESIAN_POINT('Origin',(38.4449180891584,66.3309851010726,210.6));
#36224=CARTESIAN_POINT('Origin',(36.179921252864,71.0005074807578,210.));
#36225=CARTESIAN_POINT('Origin',(19.9513700273636,43.5818784659284,213.8));
#36226=CARTESIAN_POINT('',(16.6330079023238,50.9496867315321,213.8));
#36227=CARTESIAN_POINT('Origin',(16.7328019978594,51.5413294771956,213.8));
#36228=CARTESIAN_POINT('',(27.7915336066242,49.6760211864118,213.2));
#36229=CARTESIAN_POINT('',(16.7328019978594,51.5413294771956,212.9));
#36230=CARTESIAN_POINT('Origin',(27.1246591175147,48.2938854661758,212.8));
#36231=CARTESIAN_POINT('',(27.1246591175147,48.2938854661758,212.2));
#36232=CARTESIAN_POINT('',(27.1246591175147,48.2938854661758,211.9));
#36233=CARTESIAN_POINT('Origin',(19.9513700273636,43.5818784659284,212.8));
#36234=CARTESIAN_POINT('',(20.8228154955302,48.7483603776555,212.8));
#36235=CARTESIAN_POINT('Origin',(21.0679432553689,50.2016333402581,213.2));
#36236=CARTESIAN_POINT('Origin',(16.8325960933951,52.1329722228591,212.9));
#36237=CARTESIAN_POINT('Origin',(20.8228154955302,48.7483603776555,212.2));
#36238=CARTESIAN_POINT('Origin',(27.2244532130503,48.8855282118392,211.9));
#36239=CARTESIAN_POINT('Origin',(-18.1629964860985,83.0516975441391,210.3));
#36240=CARTESIAN_POINT('Origin',(-18.1629964860985,83.0516975441391,201.3));
#36241=CARTESIAN_POINT('Origin',(-19.1740879543717,79.6651449444885,202.784409248129));
#36242=CARTESIAN_POINT('',(-15.7623923893876,80.4345282249253,213.8));
#36243=CARTESIAN_POINT('',(-15.7623923893876,80.4345282249253,202.784409248129));
#36244=CARTESIAN_POINT('',(-19.1740879543717,79.6651449444885,213.8));
#36245=CARTESIAN_POINT('',(-19.1740879543717,79.6651449444885,213.8));
#36246=CARTESIAN_POINT('',(-19.1740879543717,79.6651449444885,202.784409248129));
#36247=CARTESIAN_POINT('Origin',(-15.7623923893876,80.4345282249253,202.784409248129));
#36248=CARTESIAN_POINT('',(-14.7228500730009,83.7738348943986,213.8));
#36249=CARTESIAN_POINT('',(-14.7228500730009,83.7738348943986,202.784409248129));
#36250=CARTESIAN_POINT('',(-15.7623923893876,80.4345282249253,213.8));
#36251=CARTESIAN_POINT('Origin',(-14.7228500730009,83.7738348943986,202.784409248129));
#36252=CARTESIAN_POINT('',(-17.0950033215982,86.3437582834351,213.8));
#36253=CARTESIAN_POINT('',(-17.0950033215982,86.3437582834351,202.784409248129));
#36254=CARTESIAN_POINT('',(-14.7228500730009,83.7738348943986,213.8));
#36255=CARTESIAN_POINT('Origin',(-17.0950033215982,86.3437582834351,202.784409248129));
#36256=CARTESIAN_POINT('',(-20.5066988865823,85.5743750029983,213.8));
#36257=CARTESIAN_POINT('',(-20.5066988865823,85.5743750029983,202.784409248129));
#36258=CARTESIAN_POINT('',(-17.0950033215982,86.3437582834351,213.8));
#36259=CARTESIAN_POINT('Origin',(-20.5066988865823,85.5743750029983,202.784409248129));
#36260=CARTESIAN_POINT('',(-21.546241202969,82.235068333525,213.8));
#36261=CARTESIAN_POINT('',(-21.546241202969,82.235068333525,202.784409248129));
#36262=CARTESIAN_POINT('',(-20.5066988865823,85.5743750029983,213.8));
#36263=CARTESIAN_POINT('Origin',(-21.546241202969,82.235068333525,202.784409248129));
#36264=CARTESIAN_POINT('',(-21.546241202969,82.235068333525,213.8));
#36265=CARTESIAN_POINT('Origin',(-18.1629964860985,83.0516975441391,214.3));
#36266=CARTESIAN_POINT('',(-17.2666121411095,85.7925017674652,214.3));
#36267=CARTESIAN_POINT('',(-20.1151011495063,85.1501291478031,214.3));
#36268=CARTESIAN_POINT('',(-20.3967044277999,85.0866238174157,214.3));
#36269=CARTESIAN_POINT('',(-20.9830346463817,82.3620789942997,214.3));
#36270=CARTESIAN_POINT('',(-21.0688390561374,82.0864507363147,214.3));
#36271=CARTESIAN_POINT('',(-19.0024791348604,80.2164014604584,214.3));
#36272=CARTESIAN_POINT('',(-18.8066802663224,80.0042785328608,214.3));
#36273=CARTESIAN_POINT('',(-16.1539901264636,80.8587740801205,214.3));
#36274=CARTESIAN_POINT('',(-15.87238684817,80.9222794105078,214.3));
#36275=CARTESIAN_POINT('',(-15.2860566295882,83.6468242336239,214.3));
#36276=CARTESIAN_POINT('',(-15.2002522198325,83.9224524916089,214.3));
#36277=CARTESIAN_POINT('',(-17.4624110096475,86.0046246950628,214.3));
#36278=CARTESIAN_POINT('Origin',(-15.7091285121886,82.2877965760055,213.8));
#36279=CARTESIAN_POINT('Origin',(-16.153990126463,80.8587740801198,213.800000000001));
#36280=CARTESIAN_POINT('Origin',(-15.2860566295866,83.6468242336243,213.800000000001));
#36281=CARTESIAN_POINT('Origin',(-16.3129705205095,84.7593535478096,213.8));
#36282=CARTESIAN_POINT('Origin',(-17.2666121411088,85.7925017674677,213.800000000002));
#36283=CARTESIAN_POINT('Origin',(-17.595169633509,80.5337686991571,213.8));
#36284=CARTESIAN_POINT('Origin',(-19.0024791348609,80.2164014604572,213.800000000001));
#36285=CARTESIAN_POINT('Origin',(-18.7077916481549,85.4674963865018,213.8));
#36286=CARTESIAN_POINT('Origin',(-20.1151011495067,85.1501291478035,213.8));
#36287=CARTESIAN_POINT('Origin',(-20.0293930257817,81.328930774644,213.8));
#36288=CARTESIAN_POINT('Origin',(-20.98303464638,82.3620789943001,213.799999999999));
#36289=CARTESIAN_POINT('Origin',(-20.5381730321068,83.7911014901847,213.8));
#36290=CARTESIAN_POINT('Origin',(25.18790348116,63.761980950101,211.3));
#36291=CARTESIAN_POINT('',(21.2239277116833,64.2976077782208,211.3));
#36292=CARTESIAN_POINT('Origin',(43.0811453810944,77.1117683798101,211.));
#36293=CARTESIAN_POINT('',(44.680857697675,77.0814285680054,211.));
#36294=CARTESIAN_POINT('Origin',(43.0811453810944,77.1117683798101,211.));
#36295=CARTESIAN_POINT('Origin',(43.0811453810944,77.1117683798101,211.8));
#36296=CARTESIAN_POINT('',(44.680857697675,77.0814285680054,210.6));
#36297=CARTESIAN_POINT('',(44.680857697675,77.0814285680054,211.8));
#36298=CARTESIAN_POINT('Origin',(43.0811453810944,77.1117683798101,210.6));
#36299=CARTESIAN_POINT('Origin',(50.0785666549903,74.1079361245165,211.8));
#36300=CARTESIAN_POINT('',(47.2162408553341,75.3366668562564,210.6));
#36301=CARTESIAN_POINT('',(50.0785666549903,74.1079361245165,210.6));
#36302=CARTESIAN_POINT('',(50.0785666549903,74.1079361245165,210.6));
#36303=CARTESIAN_POINT('',(50.0785666549903,74.1079361245165,211.8));
#36304=CARTESIAN_POINT('',(50.0785666549903,74.1079361245165,211.8));
#36305=CARTESIAN_POINT('',(47.2162408553341,75.3366668562564,211.8));
#36306=CARTESIAN_POINT('',(50.0785666549903,74.1079361245165,211.8));
#36307=CARTESIAN_POINT('',(47.2162408553341,75.3366668562564,211.8));
#36308=CARTESIAN_POINT('Origin',(43.0811453810944,77.1117683798101,211.8));
#36309=CARTESIAN_POINT('',(44.9906970300894,81.1865214397907,211.8));
#36310=CARTESIAN_POINT('Origin',(43.0811453810944,77.1117683798101,211.8));
#36311=CARTESIAN_POINT('',(44.9906970300894,81.1865214397907,210.6));
#36312=CARTESIAN_POINT('',(44.9906970300894,81.1865214397907,211.8));
#36313=CARTESIAN_POINT('Origin',(43.0811453810944,77.1117683798101,210.6));
#36314=CARTESIAN_POINT('Origin',(44.9906970300894,81.1865214397907,211.8));
#36315=CARTESIAN_POINT('',(57.6817429296641,75.6575754701734,210.6));
#36316=CARTESIAN_POINT('',(44.9906970300894,81.1865214397907,210.6));
#36317=CARTESIAN_POINT('',(57.6817429296641,75.6575754701734,211.8));
#36318=CARTESIAN_POINT('',(44.9906970300894,81.1865214397907,211.8));
#36319=CARTESIAN_POINT('',(57.6817429296641,75.6575754701734,211.8));
#36320=CARTESIAN_POINT('Origin',(57.6817429296641,75.6575754701734,211.8));
#36321=CARTESIAN_POINT('',(59.0214390284855,73.5468375985269,210.6));
#36322=CARTESIAN_POINT('',(57.6817429296641,75.6575754701734,210.6));
#36323=CARTESIAN_POINT('',(59.0214390284855,73.5468375985269,211.8));
#36324=CARTESIAN_POINT('',(57.6817429296641,75.6575754701734,211.8));
#36325=CARTESIAN_POINT('',(59.0214390284855,73.5468375985269,211.8));
#36326=CARTESIAN_POINT('Origin',(59.0214390284855,73.5468375985269,211.8));
#36327=CARTESIAN_POINT('',(61.3888699102512,74.0630844855977,210.6));
#36328=CARTESIAN_POINT('',(59.0214390284855,73.5468375985269,210.6));
#36329=CARTESIAN_POINT('',(61.3888699102512,74.0630844855977,211.8));
#36330=CARTESIAN_POINT('',(59.0214390284855,73.5468375985269,211.8));
#36331=CARTESIAN_POINT('',(61.3888699102512,74.0630844855977,211.8));
#36332=CARTESIAN_POINT('Origin',(61.3888699102512,74.0630844855977,211.8));
#36333=CARTESIAN_POINT('',(60.8221863677775,72.7623289912252,210.6));
#36334=CARTESIAN_POINT('',(61.3888699102512,74.0630844855977,210.6));
#36335=CARTESIAN_POINT('',(60.8221863677775,72.7623289912252,211.8));
#36336=CARTESIAN_POINT('',(61.3888699102512,74.0630844855977,211.8));
#36337=CARTESIAN_POINT('',(60.8221863677775,72.7623289912252,211.8));
#36338=CARTESIAN_POINT('Origin',(60.8221863677775,72.7623289912252,211.8));
#36339=CARTESIAN_POINT('',(61.1303665930493,72.6323913325213,210.6));
#36340=CARTESIAN_POINT('',(60.8221863677775,72.7623289912252,210.6));
#36341=CARTESIAN_POINT('',(61.1303665930493,72.6323913325213,211.8));
#36342=CARTESIAN_POINT('',(60.8221863677775,72.7623289912252,211.8));
#36343=CARTESIAN_POINT('',(61.1303665930493,72.6323913325213,211.8));
#36344=CARTESIAN_POINT('Origin',(61.1303665930493,72.6323913325213,211.8));
#36345=CARTESIAN_POINT('',(63.4977974748151,73.148638219592,210.6));
#36346=CARTESIAN_POINT('',(61.1303665930493,72.6323913325213,210.6));
#36347=CARTESIAN_POINT('',(63.4977974748151,73.148638219592,211.8));
#36348=CARTESIAN_POINT('',(61.1303665930493,72.6323913325213,211.8));
#36349=CARTESIAN_POINT('',(63.4977974748151,73.148638219592,211.8));
#36350=CARTESIAN_POINT('Origin',(63.4977974748151,73.148638219592,211.8));
#36351=CARTESIAN_POINT('',(62.9311139323413,71.8478827252195,210.6));
#36352=CARTESIAN_POINT('',(63.4977974748151,73.148638219592,210.6));
#36353=CARTESIAN_POINT('',(62.9311139323413,71.8478827252195,211.8));
#36354=CARTESIAN_POINT('',(63.4977974748151,73.148638219592,211.8));
#36355=CARTESIAN_POINT('',(62.9311139323413,71.8478827252195,211.8));
#36356=CARTESIAN_POINT('Origin',(62.9311139323413,71.8478827252195,211.8));
#36357=CARTESIAN_POINT('',(63.2392941576131,71.7179450665156,210.6));
#36358=CARTESIAN_POINT('',(62.9311139323413,71.8478827252195,210.6));
#36359=CARTESIAN_POINT('',(63.2392941576131,71.7179450665156,211.8));
#36360=CARTESIAN_POINT('',(62.9311139323413,71.8478827252195,211.8));
#36361=CARTESIAN_POINT('',(63.2392941576131,71.7179450665156,211.8));
#36362=CARTESIAN_POINT('Origin',(63.2392941576131,71.7179450665156,211.8));
#36363=CARTESIAN_POINT('',(65.6067250393788,72.2341919535864,210.6));
#36364=CARTESIAN_POINT('',(63.2392941576131,71.7179450665156,210.6));
#36365=CARTESIAN_POINT('',(65.6067250393788,72.2341919535864,211.8));
#36366=CARTESIAN_POINT('',(63.2392941576131,71.7179450665156,211.8));
#36367=CARTESIAN_POINT('',(65.6067250393788,72.2341919535864,211.8));
#36368=CARTESIAN_POINT('Origin',(65.6067250393788,72.2341919535864,211.8));
#36369=CARTESIAN_POINT('',(65.040041496905,70.9334364592139,210.6));
#36370=CARTESIAN_POINT('',(65.6067250393788,72.2341919535864,210.6));
#36371=CARTESIAN_POINT('',(65.040041496905,70.9334364592139,211.8));
#36372=CARTESIAN_POINT('',(65.6067250393788,72.2341919535864,211.8));
#36373=CARTESIAN_POINT('',(65.040041496905,70.9334364592139,211.8));
#36374=CARTESIAN_POINT('Origin',(65.040041496905,70.9334364592139,211.8));
#36375=CARTESIAN_POINT('',(65.3482217221768,70.8034988005099,210.6));
#36376=CARTESIAN_POINT('',(65.040041496905,70.9334364592139,210.6));
#36377=CARTESIAN_POINT('',(65.3482217221768,70.8034988005099,211.8));
#36378=CARTESIAN_POINT('',(65.040041496905,70.9334364592139,211.8));
#36379=CARTESIAN_POINT('',(65.3482217221768,70.8034988005099,211.8));
#36380=CARTESIAN_POINT('Origin',(65.3482217221768,70.8034988005099,211.8));
#36381=CARTESIAN_POINT('',(67.7156526039426,71.3197456875807,210.6));
#36382=CARTESIAN_POINT('',(65.3482217221768,70.8034988005099,210.6));
#36383=CARTESIAN_POINT('',(67.7156526039426,71.3197456875807,211.8));
#36384=CARTESIAN_POINT('',(65.3482217221768,70.8034988005099,211.8));
#36385=CARTESIAN_POINT('',(67.7156526039426,71.3197456875807,211.8));
#36386=CARTESIAN_POINT('Origin',(67.7156526039426,71.3197456875807,211.8));
#36387=CARTESIAN_POINT('',(67.1489690614688,70.0189901932082,210.6));
#36388=CARTESIAN_POINT('',(67.7156526039426,71.3197456875807,210.6));
#36389=CARTESIAN_POINT('',(67.1489690614688,70.0189901932082,211.8));
#36390=CARTESIAN_POINT('',(67.7156526039426,71.3197456875807,211.8));
#36391=CARTESIAN_POINT('',(67.1489690614688,70.0189901932082,211.8));
#36392=CARTESIAN_POINT('Origin',(67.1489690614688,70.0189901932082,211.8));
#36393=CARTESIAN_POINT('',(67.4571492867406,69.8890525345043,210.6));
#36394=CARTESIAN_POINT('',(67.1489690614688,70.0189901932082,210.6));
#36395=CARTESIAN_POINT('',(67.4571492867406,69.8890525345043,211.8));
#36396=CARTESIAN_POINT('',(67.1489690614688,70.0189901932082,211.8));
#36397=CARTESIAN_POINT('',(67.4571492867406,69.8890525345043,211.8));
#36398=CARTESIAN_POINT('Origin',(67.4571492867406,69.8890525345043,211.8));
#36399=CARTESIAN_POINT('',(69.8245801685064,70.4052994215751,210.6));
#36400=CARTESIAN_POINT('',(67.4571492867406,69.8890525345043,210.6));
#36401=CARTESIAN_POINT('',(69.8245801685064,70.4052994215751,211.8));
#36402=CARTESIAN_POINT('',(67.4571492867406,69.8890525345043,211.8));
#36403=CARTESIAN_POINT('',(69.8245801685064,70.4052994215751,211.8));
#36404=CARTESIAN_POINT('Origin',(69.8245801685064,70.4052994215751,211.8));
#36405=CARTESIAN_POINT('',(69.2578966260326,69.1045439272026,210.6));
#36406=CARTESIAN_POINT('',(69.8245801685064,70.4052994215751,210.6));
#36407=CARTESIAN_POINT('',(69.2578966260326,69.1045439272026,211.8));
#36408=CARTESIAN_POINT('',(69.8245801685064,70.4052994215751,211.8));
#36409=CARTESIAN_POINT('',(69.2578966260326,69.1045439272026,211.8));
#36410=CARTESIAN_POINT('Origin',(69.2578966260326,69.1045439272026,211.8));
#36411=CARTESIAN_POINT('',(69.5660768513044,68.9746062684986,210.6));
#36412=CARTESIAN_POINT('',(69.2578966260326,69.1045439272026,210.6));
#36413=CARTESIAN_POINT('',(69.5660768513044,68.9746062684986,211.8));
#36414=CARTESIAN_POINT('',(69.2578966260326,69.1045439272026,211.8));
#36415=CARTESIAN_POINT('',(69.5660768513044,68.9746062684986,211.8));
#36416=CARTESIAN_POINT('Origin',(69.5660768513044,68.9746062684986,211.8));
#36417=CARTESIAN_POINT('',(71.9335077330702,69.4908531555695,210.6));
#36418=CARTESIAN_POINT('',(69.5660768513044,68.9746062684986,210.6));
#36419=CARTESIAN_POINT('',(71.9335077330702,69.4908531555695,211.8));
#36420=CARTESIAN_POINT('',(69.5660768513044,68.9746062684986,211.8));
#36421=CARTESIAN_POINT('',(71.9335077330702,69.4908531555695,211.8));
#36422=CARTESIAN_POINT('Origin',(71.9335077330702,69.4908531555695,211.8));
#36423=CARTESIAN_POINT('',(71.3668241905964,68.1900976611969,210.6));
#36424=CARTESIAN_POINT('',(71.9335077330702,69.4908531555695,210.6));
#36425=CARTESIAN_POINT('',(71.3668241905964,68.1900976611969,211.8));
#36426=CARTESIAN_POINT('',(71.9335077330702,69.4908531555695,211.8));
#36427=CARTESIAN_POINT('',(71.3668241905964,68.1900976611969,211.8));
#36428=CARTESIAN_POINT('Origin',(71.3668241905964,68.1900976611969,211.8));
#36429=CARTESIAN_POINT('',(71.6750044158682,68.060160002493,210.6));
#36430=CARTESIAN_POINT('',(71.3668241905964,68.1900976611969,210.6));
#36431=CARTESIAN_POINT('',(71.6750044158682,68.060160002493,211.8));
#36432=CARTESIAN_POINT('',(71.3668241905964,68.1900976611969,211.8));
#36433=CARTESIAN_POINT('',(71.6750044158682,68.060160002493,211.8));
#36434=CARTESIAN_POINT('Origin',(71.6750044158682,68.060160002493,211.8));
#36435=CARTESIAN_POINT('',(74.042435297634,68.5764068895638,210.6));
#36436=CARTESIAN_POINT('',(71.6750044158682,68.060160002493,210.6));
#36437=CARTESIAN_POINT('',(74.042435297634,68.5764068895638,211.8));
#36438=CARTESIAN_POINT('',(71.6750044158682,68.060160002493,211.8));
#36439=CARTESIAN_POINT('',(74.042435297634,68.5764068895638,211.8));
#36440=CARTESIAN_POINT('Origin',(74.042435297634,68.5764068895638,211.8));
#36441=CARTESIAN_POINT('',(73.4757517551602,67.2756513951913,210.6));
#36442=CARTESIAN_POINT('',(74.042435297634,68.5764068895638,210.6));
#36443=CARTESIAN_POINT('',(73.4757517551602,67.2756513951913,211.8));
#36444=CARTESIAN_POINT('',(74.042435297634,68.5764068895638,211.8));
#36445=CARTESIAN_POINT('',(73.4757517551602,67.2756513951913,211.8));
#36446=CARTESIAN_POINT('Origin',(73.4757517551602,67.2756513951913,211.8));
#36447=CARTESIAN_POINT('',(73.783931980432,67.1457137364874,210.6));
#36448=CARTESIAN_POINT('',(73.4757517551602,67.2756513951913,210.6));
#36449=CARTESIAN_POINT('',(73.783931980432,67.1457137364874,211.8));
#36450=CARTESIAN_POINT('',(73.4757517551602,67.2756513951913,211.8));
#36451=CARTESIAN_POINT('',(73.783931980432,67.1457137364874,211.8));
#36452=CARTESIAN_POINT('Origin',(73.783931980432,67.1457137364874,211.8));
#36453=CARTESIAN_POINT('',(76.1513628621978,67.6619606235582,210.6));
#36454=CARTESIAN_POINT('',(73.783931980432,67.1457137364874,210.6));
#36455=CARTESIAN_POINT('',(76.1513628621978,67.6619606235582,211.8));
#36456=CARTESIAN_POINT('',(73.783931980432,67.1457137364874,211.8));
#36457=CARTESIAN_POINT('',(76.1513628621978,67.6619606235582,211.8));
#36458=CARTESIAN_POINT('Origin',(76.1513628621978,67.6619606235582,211.8));
#36459=CARTESIAN_POINT('',(75.584679319724,66.3612051291856,210.6));
#36460=CARTESIAN_POINT('',(76.1513628621978,67.6619606235582,210.6));
#36461=CARTESIAN_POINT('',(75.584679319724,66.3612051291856,211.8));
#36462=CARTESIAN_POINT('',(76.1513628621978,67.6619606235582,211.8));
#36463=CARTESIAN_POINT('',(75.584679319724,66.3612051291856,211.8));
#36464=CARTESIAN_POINT('Origin',(75.584679319724,66.3612051291856,211.8));
#36465=CARTESIAN_POINT('',(75.8928595449958,66.2312674704817,210.6));
#36466=CARTESIAN_POINT('',(75.584679319724,66.3612051291856,210.6));
#36467=CARTESIAN_POINT('',(75.8928595449958,66.2312674704817,211.8));
#36468=CARTESIAN_POINT('',(75.584679319724,66.3612051291856,211.8));
#36469=CARTESIAN_POINT('',(75.8928595449958,66.2312674704817,211.8));
#36470=CARTESIAN_POINT('Origin',(75.8928595449958,66.2312674704817,211.8));
#36471=CARTESIAN_POINT('',(78.2602904267616,66.7475143575525,210.6));
#36472=CARTESIAN_POINT('',(75.8928595449958,66.2312674704817,210.6));
#36473=CARTESIAN_POINT('',(78.2602904267616,66.7475143575525,211.8));
#36474=CARTESIAN_POINT('',(75.8928595449958,66.2312674704817,211.8));
#36475=CARTESIAN_POINT('',(78.2602904267616,66.7475143575525,211.8));
#36476=CARTESIAN_POINT('Origin',(78.2602904267616,66.7475143575525,211.8));
#36477=CARTESIAN_POINT('',(77.6936068842878,65.44675886318,210.6));
#36478=CARTESIAN_POINT('',(78.2602904267616,66.7475143575525,210.6));
#36479=CARTESIAN_POINT('',(77.6936068842878,65.44675886318,211.8));
#36480=CARTESIAN_POINT('',(78.2602904267616,66.7475143575525,211.8));
#36481=CARTESIAN_POINT('',(77.6936068842878,65.44675886318,211.8));
#36482=CARTESIAN_POINT('Origin',(77.6936068842878,65.44675886318,211.8));
#36483=CARTESIAN_POINT('',(78.0017871095596,65.3168212044761,210.6));
#36484=CARTESIAN_POINT('',(77.6936068842878,65.44675886318,210.6));
#36485=CARTESIAN_POINT('',(78.0017871095596,65.3168212044761,211.8));
#36486=CARTESIAN_POINT('',(77.6936068842878,65.44675886318,211.8));
#36487=CARTESIAN_POINT('',(78.0017871095596,65.3168212044761,211.8));
#36488=CARTESIAN_POINT('Origin',(78.0017871095596,65.3168212044761,211.8));
#36489=CARTESIAN_POINT('',(80.3692179913253,65.8330680915469,210.6));
#36490=CARTESIAN_POINT('',(78.0017871095596,65.3168212044761,210.6));
#36491=CARTESIAN_POINT('',(80.3692179913253,65.8330680915469,211.8));
#36492=CARTESIAN_POINT('',(78.0017871095596,65.3168212044761,211.8));
#36493=CARTESIAN_POINT('',(80.3692179913253,65.8330680915469,211.8));
#36494=CARTESIAN_POINT('Origin',(80.3692179913253,65.8330680915469,211.8));
#36495=CARTESIAN_POINT('',(79.8025344488516,64.5323125971744,210.6));
#36496=CARTESIAN_POINT('',(80.3692179913253,65.8330680915469,210.6));
#36497=CARTESIAN_POINT('',(79.8025344488516,64.5323125971744,211.8));
#36498=CARTESIAN_POINT('',(80.3692179913253,65.8330680915469,211.8));
#36499=CARTESIAN_POINT('',(79.8025344488516,64.5323125971744,211.8));
#36500=CARTESIAN_POINT('Origin',(79.8025344488516,64.5323125971744,211.8));
#36501=CARTESIAN_POINT('',(80.1107146741234,64.4023749384704,210.6));
#36502=CARTESIAN_POINT('',(79.8025344488516,64.5323125971744,210.6));
#36503=CARTESIAN_POINT('',(80.1107146741234,64.4023749384704,211.8));
#36504=CARTESIAN_POINT('',(79.8025344488516,64.5323125971744,211.8));
#36505=CARTESIAN_POINT('',(80.1107146741234,64.4023749384704,211.8));
#36506=CARTESIAN_POINT('Origin',(80.1107146741234,64.4023749384704,211.8));
#36507=CARTESIAN_POINT('',(82.4781455558892,64.9186218255412,210.6));
#36508=CARTESIAN_POINT('',(80.1107146741234,64.4023749384704,210.6));
#36509=CARTESIAN_POINT('',(82.4781455558892,64.9186218255412,211.8));
#36510=CARTESIAN_POINT('',(80.1107146741234,64.4023749384704,211.8));
#36511=CARTESIAN_POINT('',(82.4781455558892,64.9186218255412,211.8));
#36512=CARTESIAN_POINT('Origin',(82.4781455558892,64.9186218255412,211.8));
#36513=CARTESIAN_POINT('',(81.9114620134154,63.6178663311687,210.6));
#36514=CARTESIAN_POINT('',(82.4781455558892,64.9186218255412,210.6));
#36515=CARTESIAN_POINT('',(81.9114620134154,63.6178663311687,211.8));
#36516=CARTESIAN_POINT('',(82.4781455558892,64.9186218255412,211.8));
#36517=CARTESIAN_POINT('',(81.9114620134154,63.6178663311687,211.8));
#36518=CARTESIAN_POINT('Origin',(81.9114620134154,63.6178663311687,211.8));
#36519=CARTESIAN_POINT('',(82.2196422386872,63.4879286724648,210.6));
#36520=CARTESIAN_POINT('',(81.9114620134154,63.6178663311687,210.6));
#36521=CARTESIAN_POINT('',(82.2196422386872,63.4879286724648,211.8));
#36522=CARTESIAN_POINT('',(81.9114620134154,63.6178663311687,211.8));
#36523=CARTESIAN_POINT('',(82.2196422386872,63.4879286724648,211.8));
#36524=CARTESIAN_POINT('Origin',(82.2196422386872,63.4879286724648,211.8));
#36525=CARTESIAN_POINT('',(84.5870731204529,64.0041755595356,210.6));
#36526=CARTESIAN_POINT('',(82.2196422386872,63.4879286724648,210.6));
#36527=CARTESIAN_POINT('',(84.5870731204529,64.0041755595356,211.8));
#36528=CARTESIAN_POINT('',(82.2196422386872,63.4879286724648,211.8));
#36529=CARTESIAN_POINT('',(84.5870731204529,64.0041755595356,211.8));
#36530=CARTESIAN_POINT('Origin',(84.5870731204529,64.0041755595356,211.8));
#36531=CARTESIAN_POINT('',(84.0203895779791,62.7034200651631,210.6));
#36532=CARTESIAN_POINT('',(84.5870731204529,64.0041755595356,210.6));
#36533=CARTESIAN_POINT('',(84.0203895779791,62.7034200651631,211.8));
#36534=CARTESIAN_POINT('',(84.5870731204529,64.0041755595356,211.8));
#36535=CARTESIAN_POINT('',(84.0203895779791,62.7034200651631,211.8));
#36536=CARTESIAN_POINT('Origin',(84.0203895779791,62.7034200651631,211.8));
#36537=CARTESIAN_POINT('',(84.983313171664,62.2363592862195,210.6));
#36538=CARTESIAN_POINT('',(84.0203895779791,62.7034200651631,210.6));
#36539=CARTESIAN_POINT('',(84.983313171664,62.2363592862195,211.8));
#36540=CARTESIAN_POINT('',(84.0203895779791,62.7034200651631,211.8));
#36541=CARTESIAN_POINT('',(84.983313171664,62.2363592862195,211.8));
#36542=CARTESIAN_POINT('Origin',(81.1139782547789,63.6271067952341,211.8));
#36543=CARTESIAN_POINT('',(79.6224513102927,59.7954911168644,210.6));
#36544=CARTESIAN_POINT('Origin',(81.1139782547789,63.6271067952341,210.6));
#36545=CARTESIAN_POINT('',(79.6224513102927,59.7954911168644,211.8));
#36546=CARTESIAN_POINT('Origin',(81.1139782547789,63.6271067952341,211.8));
#36547=CARTESIAN_POINT('',(79.6224513102927,59.7954911168644,211.8));
#36548=CARTESIAN_POINT('Origin',(79.6224513102927,59.7954911168644,211.8));
#36549=CARTESIAN_POINT('',(52.2391399600025,71.7252288329682,210.6));
#36550=CARTESIAN_POINT('',(79.6224513102927,59.7954911168644,210.6));
#36551=CARTESIAN_POINT('',(52.2391399600025,71.7252288329682,211.8));
#36552=CARTESIAN_POINT('',(79.6224513102927,59.7954911168644,211.8));
#36553=CARTESIAN_POINT('',(52.2391399600025,71.7252288329682,211.8));
#36554=CARTESIAN_POINT('Origin',(52.2391399600025,71.7252288329682,211.8));
#36555=CARTESIAN_POINT('',(52.2391399600025,71.7252288329682,210.6));
#36556=CARTESIAN_POINT('',(52.2391399600025,71.7252288329682,211.8));
#36557=CARTESIAN_POINT('Origin',(43.0811453810944,77.1117683798101,210.6));
#36558=CARTESIAN_POINT('Origin',(43.0811453810944,77.1117683798101,211.8));
#36559=CARTESIAN_POINT('Origin',(43.0811453810944,77.1117683798101,212.));
#36560=CARTESIAN_POINT('',(0.,0.,0.));
#36561=CARTESIAN_POINT('Origin',(19.9513700273636,43.5818784659284,216.094898865397));
#36562=CARTESIAN_POINT('',(21.4430958752503,43.5818784659284,209.094898865397));
#36563=CARTESIAN_POINT('Origin',(19.9513700273636,43.5818784659284,209.094898865397));
#36564=CARTESIAN_POINT('',(21.4430958752503,43.5818784659284,208.094898865397));
#36565=CARTESIAN_POINT('',(21.4430958752503,43.5818784659284,216.094898865397));
#36566=CARTESIAN_POINT('Origin',(19.9513700273636,43.5818784659284,208.094898865397));
#36567=CARTESIAN_POINT('Origin',(24.6430224985391,43.5386624163653,208.094898865397));
#36568=CARTESIAN_POINT('',(24.6430224985391,43.5386624163653,209.094898865397));
#36569=CARTESIAN_POINT('',(24.7923296637165,39.1253694570289,209.094898865397));
#36570=CARTESIAN_POINT('',(24.6430224985391,43.5386624163653,209.094898865397));
#36571=CARTESIAN_POINT('',(24.7923296637165,39.1253694570289,208.094898865397));
#36572=CARTESIAN_POINT('',(24.7923296637165,39.1253694570289,208.094898865397));
#36573=CARTESIAN_POINT('',(24.6430224985391,43.5386624163653,208.094898865397));
#36574=CARTESIAN_POINT('',(24.6430224985391,43.5386624163653,208.094898865397));
#36575=CARTESIAN_POINT('',(24.6430224985391,43.5386624163653,208.094898865397));
#36576=CARTESIAN_POINT('Origin',(19.951370027377,43.5818784659222,208.094898865397));
#36577=CARTESIAN_POINT('',(15.2632338299238,43.7685587574091,208.094898865397));
#36578=CARTESIAN_POINT('Origin',(19.951370027377,43.5818784659222,208.094898865397));
#36579=CARTESIAN_POINT('',(15.2632338299238,43.7685587574091,209.094898865397));
#36580=CARTESIAN_POINT('',(15.2632338299238,43.7685587574091,208.094898865397));
#36581=CARTESIAN_POINT('Origin',(19.951370027377,43.5818784659222,209.094898865397));
#36582=CARTESIAN_POINT('Origin',(15.2976067234458,42.7525482478522,208.094898865397));
#36583=CARTESIAN_POINT('',(15.2976067234458,42.7525482478522,209.094898865397));
#36584=CARTESIAN_POINT('',(15.2976067234458,42.7525482478522,209.094898865397));
#36585=CARTESIAN_POINT('',(15.2976067234458,42.7525482478522,208.094898865397));
#36586=CARTESIAN_POINT('',(15.2976067234458,42.7525482478522,208.094898865397));
#36587=CARTESIAN_POINT('',(15.2976067234458,42.7525482478522,208.094898865397));
#36588=CARTESIAN_POINT('Origin',(-2.17548604454373,39.6387319900736,208.094898865397));
#36589=CARTESIAN_POINT('',(-12.4435067339657,37.8089053999865,209.094898865397));
#36590=CARTESIAN_POINT('',(-2.17548604454373,39.6387319900736,209.094898865397));
#36591=CARTESIAN_POINT('',(-12.4435067339657,37.8089053999865,208.094898865397));
#36592=CARTESIAN_POINT('',(-12.4435067339657,37.8089053999865,208.094898865397));
#36593=CARTESIAN_POINT('',(-12.4435067339657,37.8089053999865,208.094898865397));
#36594=CARTESIAN_POINT('Origin',(-20.1379345336707,35.2639251777624,208.094898865397));
#36595=CARTESIAN_POINT('',(-20.1379345336707,35.2639251777624,209.094898865397));
#36596=CARTESIAN_POINT('',(-20.1379345336707,35.2639251777624,209.094898865397));
#36597=CARTESIAN_POINT('',(-20.1379345336707,35.2639251777624,208.094898865397));
#36598=CARTESIAN_POINT('',(-20.1379345336707,35.2639251777624,208.094898865397));
#36599=CARTESIAN_POINT('',(-20.1379345336707,35.2639251777624,208.094898865397));
#36600=CARTESIAN_POINT('Origin',(-20.0067099032547,31.3851244730677,208.094898865397));
#36601=CARTESIAN_POINT('',(-20.0067099032547,31.3851244730677,209.094898865397));
#36602=CARTESIAN_POINT('',(-20.0067099032547,31.3851244730677,209.094898865397));
#36603=CARTESIAN_POINT('',(-20.0067099032547,31.3851244730677,208.094898865397));
#36604=CARTESIAN_POINT('',(-20.0067099032547,31.3851244730677,208.094898865397));
#36605=CARTESIAN_POINT('',(-20.0067099032547,31.3851244730677,208.094898865397));
#36606=CARTESIAN_POINT('Origin',(-19.7470473101411,31.6024131357033,208.094898865397));
#36607=CARTESIAN_POINT('',(-19.6054127952646,31.2948766510902,209.094898865397));
#36608=CARTESIAN_POINT('Origin',(-19.7470473101411,31.6024131357033,209.094898865397));
#36609=CARTESIAN_POINT('',(-19.6054127952646,31.2948766510902,208.094898865397));
#36610=CARTESIAN_POINT('Origin',(-19.7470473101411,31.6024131357033,208.094898865397));
#36611=CARTESIAN_POINT('',(-19.6054127952646,31.2948766510902,208.094898865397));
#36612=CARTESIAN_POINT('Origin',(-14.2756540048791,33.64109670922,208.094898865397));
#36613=CARTESIAN_POINT('',(-14.2756540048791,33.64109670922,209.094898865397));
#36614=CARTESIAN_POINT('',(-14.2756540048791,33.64109670922,209.094898865397));
#36615=CARTESIAN_POINT('',(-14.2756540048791,33.64109670922,208.094898865397));
#36616=CARTESIAN_POINT('',(-14.2756540048791,33.64109670922,208.094898865397));
#36617=CARTESIAN_POINT('',(-14.2756540048791,33.64109670922,208.094898865397));
#36618=CARTESIAN_POINT('Origin',(-12.364689956501,35.5264570920893,208.094898865397));
#36619=CARTESIAN_POINT('',(-12.364689956501,35.5264570920893,209.094898865397));
#36620=CARTESIAN_POINT('',(-12.364689956501,35.5264570920893,209.094898865397));
#36621=CARTESIAN_POINT('',(-12.364689956501,35.5264570920893,208.094898865397));
#36622=CARTESIAN_POINT('',(-12.364689956501,35.5264570920893,208.094898865397));
#36623=CARTESIAN_POINT('',(-12.364689956501,35.5264570920893,208.094898865397));
#36624=CARTESIAN_POINT('Origin',(22.3452540862996,36.7007374755235,208.094898865397));
#36625=CARTESIAN_POINT('',(22.3452540862996,36.7007374755235,209.094898865397));
#36626=CARTESIAN_POINT('',(22.3452540862996,36.7007374755235,209.094898865397));
#36627=CARTESIAN_POINT('',(22.3452540862996,36.7007374755235,208.094898865397));
#36628=CARTESIAN_POINT('',(22.3452540862996,36.7007374755235,208.094898865397));
#36629=CARTESIAN_POINT('',(22.3452540862996,36.7007374755235,208.094898865397));
#36630=CARTESIAN_POINT('Origin',(22.0034443343711,39.4928906399508,208.094898865397));
#36631=CARTESIAN_POINT('Origin',(22.0034443343711,39.4928906399508,209.094898865397));
#36632=CARTESIAN_POINT('Origin',(22.0034443343711,39.4928906399508,208.094898865397));
#36633=CARTESIAN_POINT('Origin',(22.0034443343711,39.4928906399508,209.094898865397));
#36634=CARTESIAN_POINT('Origin',(22.0034443343711,39.4928906399508,208.094898865397));
#36635=CARTESIAN_POINT('',(0.,0.,0.));
#36636=CARTESIAN_POINT('',(0.,0.,0.));
#36637=CARTESIAN_POINT('',(0.,0.,0.));
#36638=CARTESIAN_POINT('',(0.,0.,0.));
#36639=CARTESIAN_POINT('',(0.,0.,0.));
#36640=CARTESIAN_POINT('',(0.,0.,0.));
#36641=CARTESIAN_POINT('',(0.,0.,0.));
#36642=CARTESIAN_POINT('',(0.,0.,0.));
#36643=CARTESIAN_POINT('',(0.,0.,0.));
#36644=CARTESIAN_POINT('',(0.,0.,0.));
#36645=UNCERTAINTY_MEASURE_WITH_UNIT(LENGTH_MEASURE(0.01),#36669,
'DISTANCE_ACCURACY_VALUE',
'Maximum model space distance between geometric entities at asserted c
onnectivities');
#36646=UNCERTAINTY_MEASURE_WITH_UNIT(LENGTH_MEASURE(0.01),#36669,
'DISTANCE_ACCURACY_VALUE',
'Maximum model space distance between geometric entities at asserted c
onnectivities');
#36647=UNCERTAINTY_MEASURE_WITH_UNIT(LENGTH_MEASURE(0.01),#36669,
'DISTANCE_ACCURACY_VALUE',
'Maximum model space distance between geometric entities at asserted c
onnectivities');
#36648=UNCERTAINTY_MEASURE_WITH_UNIT(LENGTH_MEASURE(0.01),#36669,
'DISTANCE_ACCURACY_VALUE',
'Maximum model space distance between geometric entities at asserted c
onnectivities');
#36649=UNCERTAINTY_MEASURE_WITH_UNIT(LENGTH_MEASURE(0.01),#36669,
'DISTANCE_ACCURACY_VALUE',
'Maximum model space distance between geometric entities at asserted c
onnectivities');
#36650=UNCERTAINTY_MEASURE_WITH_UNIT(LENGTH_MEASURE(0.01),#36669,
'DISTANCE_ACCURACY_VALUE',
'Maximum model space distance between geometric entities at asserted c
onnectivities');
#36651=UNCERTAINTY_MEASURE_WITH_UNIT(LENGTH_MEASURE(0.01),#36669,
'DISTANCE_ACCURACY_VALUE',
'Maximum model space distance between geometric entities at asserted c
onnectivities');
#36652=UNCERTAINTY_MEASURE_WITH_UNIT(LENGTH_MEASURE(0.01),#36669,
'DISTANCE_ACCURACY_VALUE',
'Maximum model space distance between geometric entities at asserted c
onnectivities');
#36653=UNCERTAINTY_MEASURE_WITH_UNIT(LENGTH_MEASURE(0.01),#36669,
'DISTANCE_ACCURACY_VALUE',
'Maximum model space distance between geometric entities at asserted c
onnectivities');
#36654=UNCERTAINTY_MEASURE_WITH_UNIT(LENGTH_MEASURE(0.01),#36669,
'DISTANCE_ACCURACY_VALUE',
'Maximum model space distance between geometric entities at asserted c
onnectivities');
#36655=UNCERTAINTY_MEASURE_WITH_UNIT(LENGTH_MEASURE(0.01),#36669,
'DISTANCE_ACCURACY_VALUE',
'Maximum model space distance between geometric entities at asserted c
onnectivities');
#36656=UNCERTAINTY_MEASURE_WITH_UNIT(LENGTH_MEASURE(0.01),#36669,
'DISTANCE_ACCURACY_VALUE',
'Maximum model space distance between geometric entities at asserted c
onnectivities');
#36657=(
GEOMETRIC_REPRESENTATION_CONTEXT(3)
GLOBAL_UNCERTAINTY_ASSIGNED_CONTEXT((#36645))
GLOBAL_UNIT_ASSIGNED_CONTEXT((#36669,#36671,#36672))
REPRESENTATION_CONTEXT('','3D')
);
#36658=(
GEOMETRIC_REPRESENTATION_CONTEXT(3)
GLOBAL_UNCERTAINTY_ASSIGNED_CONTEXT((#36646))
GLOBAL_UNIT_ASSIGNED_CONTEXT((#36669,#36671,#36672))
REPRESENTATION_CONTEXT('','3D')
);
#36659=(
GEOMETRIC_REPRESENTATION_CONTEXT(3)
GLOBAL_UNCERTAINTY_ASSIGNED_CONTEXT((#36647))
GLOBAL_UNIT_ASSIGNED_CONTEXT((#36669,#36671,#36672))
REPRESENTATION_CONTEXT('','3D')
);
#36660=(
GEOMETRIC_REPRESENTATION_CONTEXT(3)
GLOBAL_UNCERTAINTY_ASSIGNED_CONTEXT((#36648))
GLOBAL_UNIT_ASSIGNED_CONTEXT((#36669,#36671,#36672))
REPRESENTATION_CONTEXT('','3D')
);
#36661=(
GEOMETRIC_REPRESENTATION_CONTEXT(3)
GLOBAL_UNCERTAINTY_ASSIGNED_CONTEXT((#36649))
GLOBAL_UNIT_ASSIGNED_CONTEXT((#36669,#36671,#36672))
REPRESENTATION_CONTEXT('','3D')
);
#36662=(
GEOMETRIC_REPRESENTATION_CONTEXT(3)
GLOBAL_UNCERTAINTY_ASSIGNED_CONTEXT((#36650))
GLOBAL_UNIT_ASSIGNED_CONTEXT((#36669,#36671,#36672))
REPRESENTATION_CONTEXT('','3D')
);
#36663=(
GEOMETRIC_REPRESENTATION_CONTEXT(3)
GLOBAL_UNCERTAINTY_ASSIGNED_CONTEXT((#36651))
GLOBAL_UNIT_ASSIGNED_CONTEXT((#36669,#36671,#36672))
REPRESENTATION_CONTEXT('','3D')
);
#36664=(
GEOMETRIC_REPRESENTATION_CONTEXT(3)
GLOBAL_UNCERTAINTY_ASSIGNED_CONTEXT((#36652))
GLOBAL_UNIT_ASSIGNED_CONTEXT((#36669,#36671,#36672))
REPRESENTATION_CONTEXT('','3D')
);
#36665=(
GEOMETRIC_REPRESENTATION_CONTEXT(3)
GLOBAL_UNCERTAINTY_ASSIGNED_CONTEXT((#36653))
GLOBAL_UNIT_ASSIGNED_CONTEXT((#36669,#36671,#36672))
REPRESENTATION_CONTEXT('','3D')
);
#36666=(
GEOMETRIC_REPRESENTATION_CONTEXT(3)
GLOBAL_UNCERTAINTY_ASSIGNED_CONTEXT((#36654))
GLOBAL_UNIT_ASSIGNED_CONTEXT((#36669,#36671,#36672))
REPRESENTATION_CONTEXT('','3D')
);
#36667=(
GEOMETRIC_REPRESENTATION_CONTEXT(3)
GLOBAL_UNCERTAINTY_ASSIGNED_CONTEXT((#36655))
GLOBAL_UNIT_ASSIGNED_CONTEXT((#36669,#36671,#36672))
REPRESENTATION_CONTEXT('','3D')
);
#36668=(
GEOMETRIC_REPRESENTATION_CONTEXT(3)
GLOBAL_UNCERTAINTY_ASSIGNED_CONTEXT((#36656))
GLOBAL_UNIT_ASSIGNED_CONTEXT((#36669,#36671,#36672))
REPRESENTATION_CONTEXT('','3D')
);
#36669=(
LENGTH_UNIT()
NAMED_UNIT(*)
SI_UNIT(.MILLI.,.METRE.)
);
#36670=(
LENGTH_UNIT()
NAMED_UNIT(*)
SI_UNIT($,.METRE.)
);
#36671=(
NAMED_UNIT(*)
PLANE_ANGLE_UNIT()
SI_UNIT($,.RADIAN.)
);
#36672=(
NAMED_UNIT(*)
SI_UNIT($,.STERADIAN.)
SOLID_ANGLE_UNIT()
);
#36673=SHAPE_DEFINITION_REPRESENTATION(#36684,#36705);
#36674=SHAPE_DEFINITION_REPRESENTATION(#36685,#36706);
#36675=SHAPE_DEFINITION_REPRESENTATION(#36686,#36707);
#36676=SHAPE_DEFINITION_REPRESENTATION(#36687,#36708);
#36677=SHAPE_DEFINITION_REPRESENTATION(#36688,#36709);
#36678=SHAPE_DEFINITION_REPRESENTATION(#36689,#36710);
#36679=SHAPE_DEFINITION_REPRESENTATION(#36690,#36711);
#36680=SHAPE_DEFINITION_REPRESENTATION(#36691,#36712);
#36681=SHAPE_DEFINITION_REPRESENTATION(#36692,#36713);
#36682=SHAPE_DEFINITION_REPRESENTATION(#36693,#36714);
#36683=SHAPE_DEFINITION_REPRESENTATION(#36694,#36715);
#36684=PRODUCT_DEFINITION_SHAPE('',$,#36717);
#36685=PRODUCT_DEFINITION_SHAPE('',$,#36718);
#36686=PRODUCT_DEFINITION_SHAPE('',$,#36719);
#36687=PRODUCT_DEFINITION_SHAPE('',$,#36720);
#36688=PRODUCT_DEFINITION_SHAPE('',$,#36721);
#36689=PRODUCT_DEFINITION_SHAPE('',$,#36722);
#36690=PRODUCT_DEFINITION_SHAPE('',$,#36723);
#36691=PRODUCT_DEFINITION_SHAPE('',$,#36724);
#36692=PRODUCT_DEFINITION_SHAPE('',$,#36725);
#36693=PRODUCT_DEFINITION_SHAPE('',$,#36726);
#36694=PRODUCT_DEFINITION_SHAPE('',$,#36727);
#36695=PRODUCT_DEFINITION_SHAPE($,$,#41);
#36696=PRODUCT_DEFINITION_SHAPE($,$,#42);
#36697=PRODUCT_DEFINITION_SHAPE($,$,#43);
#36698=PRODUCT_DEFINITION_SHAPE($,$,#44);
#36699=PRODUCT_DEFINITION_SHAPE($,$,#45);
#36700=PRODUCT_DEFINITION_SHAPE($,$,#46);
#36701=PRODUCT_DEFINITION_SHAPE($,$,#47);
#36702=PRODUCT_DEFINITION_SHAPE($,$,#48);
#36703=PRODUCT_DEFINITION_SHAPE($,$,#49);
#36704=PRODUCT_DEFINITION_SHAPE($,$,#50);
#36705=SHAPE_REPRESENTATION('',(#17915,#19428,#19429,#19430,#19431,#19432,
#19433,#19434,#19435,#19436,#19437),#36657);
#36706=SHAPE_REPRESENTATION('',(#17916),#36658);
#36707=SHAPE_REPRESENTATION('',(#18105),#36659);
#36708=SHAPE_REPRESENTATION('',(#18270),#36660);
#36709=SHAPE_REPRESENTATION('',(#18564),#36661);
#36710=SHAPE_REPRESENTATION('',(#18726),#36662);
#36711=SHAPE_REPRESENTATION('',(#18755),#36663);
#36712=SHAPE_REPRESENTATION('',(#18787),#36664);
#36713=SHAPE_REPRESENTATION('',(#19085),#36665);
#36714=SHAPE_REPRESENTATION('',(#19168),#36666);
#36715=SHAPE_REPRESENTATION('',(#19405),#36667);
#36716=PRODUCT_DEFINITION_CONTEXT('part definition',#36751,'design');
#36717=PRODUCT_DEFINITION('MAS-177 Tape and Reel Feeder',
'TAS-002',#36728,#36716);
#36718=PRODUCT_DEFINITION('Tape','Tape',#36729,#36716);
#36719=PRODUCT_DEFINITION('Component Pick Up Window Plate',
'Component Pick Up Window Plate',#36730,#36716);
#36720=PRODUCT_DEFINITION('Cover Tape Peel Off Spool',
'Cover Tape Peel Off Spool',#36731,#36716);
#36721=PRODUCT_DEFINITION('Feed Head Aluminum Chassis',
'Feed Head Aluminum Chassis',#36732,#36716);
#36722=PRODUCT_DEFINITION('Tape Feed Drive Shaft Motor',
'Tape Feed Drive Shaft Motor',#36733,#36716);
#36723=PRODUCT_DEFINITION('Feed Track Steel Guide Channel',
'Feed Track Steel Guide Channel',#36734,#36716);
#36724=PRODUCT_DEFINITION('Sprocket Tape Drive Gear',
'Sprocket Tape Drive Gear',#36735,#36716);
#36725=PRODUCT_DEFINITION('Optical Tape Sensor Mount',
'Optical Tape Sensor Mount',#36736,#36716);
#36726=PRODUCT_DEFINITION('Tensioner Lever Arm','Tensioner Lever Arm',#36737,
#36716);
#36727=PRODUCT_DEFINITION('Ratchet Indexing Pawl',
'Ratchet Indexing Pawl',#36738,#36716);
#36728=PRODUCT_DEFINITION_FORMATION('',$,#36753);
#36729=PRODUCT_DEFINITION_FORMATION('',$,#36754);
#36730=PRODUCT_DEFINITION_FORMATION('',$,#36755);
#36731=PRODUCT_DEFINITION_FORMATION('',$,#36756);
#36732=PRODUCT_DEFINITION_FORMATION('',$,#36757);
#36733=PRODUCT_DEFINITION_FORMATION('',$,#36758);
#36734=PRODUCT_DEFINITION_FORMATION('',$,#36759);
#36735=PRODUCT_DEFINITION_FORMATION('',$,#36760);
#36736=PRODUCT_DEFINITION_FORMATION('',$,#36761);
#36737=PRODUCT_DEFINITION_FORMATION('',$,#36762);
#36738=PRODUCT_DEFINITION_FORMATION('',$,#36763);
#36739=PRODUCT_RELATED_PRODUCT_CATEGORY(
'TAS-002',
'TAS-002',(#36753));
#36740=PRODUCT_RELATED_PRODUCT_CATEGORY('Tape','Tape',(#36754));
#36741=PRODUCT_RELATED_PRODUCT_CATEGORY(
'Component Pick Up Window Plate','Component Pick Up Window Plate',(#36755));
#36742=PRODUCT_RELATED_PRODUCT_CATEGORY('Cover Tape Peel Off Spool',
'Cover Tape Peel Off Spool',(#36756));
#36743=PRODUCT_RELATED_PRODUCT_CATEGORY('Feed Head Aluminum Chassis',
'Feed Head Aluminum Chassis',(#36757));
#36744=PRODUCT_RELATED_PRODUCT_CATEGORY('Tape Feed Drive Shaft Motor',
'Tape Feed Drive Shaft Motor',(#36758));
#36745=PRODUCT_RELATED_PRODUCT_CATEGORY(
'Feed Track Steel Guide Channel','Feed Track Steel Guide Channel',(#36759));
#36746=PRODUCT_RELATED_PRODUCT_CATEGORY('Sprocket Tape Drive Gear',
'Sprocket Tape Drive Gear',(#36760));
#36747=PRODUCT_RELATED_PRODUCT_CATEGORY('Optical Tape Sensor Mount',
'Optical Tape Sensor Mount',(#36761));
#36748=PRODUCT_RELATED_PRODUCT_CATEGORY('Tensioner Lever Arm',
'Tensioner Lever Arm',(#36762));
#36749=PRODUCT_RELATED_PRODUCT_CATEGORY('Ratchet Indexing Pawl',
'Ratchet Indexing Pawl',(#36763));
#36750=APPLICATION_PROTOCOL_DEFINITION('international standard',
'automotive_design',2009,#36751);
#36751=APPLICATION_CONTEXT(
'Core Data for Automotive Mechanical Design Process');
#36752=PRODUCT_CONTEXT('part definition',#36751,'mechanical');
#36753=PRODUCT('MAS-177 Tape and Reel Feeder',
'TAS-002','STEP AP214',(#36752));
#36754=PRODUCT('Tape','Tape',$,(#36752));
#36755=PRODUCT('Component Pick Up Window Plate',
'Component Pick Up Window Plate',$,(#36752));
#36756=PRODUCT('Cover Tape Peel Off Spool','Cover Tape Peel Off Spool',
$,(#36752));
#36757=PRODUCT('Feed Head Aluminum Chassis',
'Feed Head Aluminum Chassis',$,(#36752));
#36758=PRODUCT('Tape Feed Drive Shaft Motor',
'Tape Feed Drive Shaft Motor',$,(#36752));
#36759=PRODUCT('Feed Track Steel Guide Channel',
'Feed Track Steel Guide Channel',$,(#36752));
#36760=PRODUCT('Sprocket Tape Drive Gear','Sprocket Tape Drive Gear',$,
(#36752));
#36761=PRODUCT('Optical Tape Sensor Mount','Optical Tape Sensor Mount',
$,(#36752));
#36762=PRODUCT('Tensioner Lever Arm','Tensioner Lever Arm',$,(#36752));
#36763=PRODUCT('Ratchet Indexing Pawl','Ratchet Indexing Pawl',$,(#36752));
#36764=PRESENTATION_STYLE_ASSIGNMENT((#36771));
#36765=PRESENTATION_STYLE_ASSIGNMENT((#36772));
#36766=PRESENTATION_STYLE_ASSIGNMENT((#36773));
#36767=PRESENTATION_STYLE_ASSIGNMENT((#36774));
#36768=PRESENTATION_STYLE_ASSIGNMENT((#36775));
#36769=PRESENTATION_STYLE_ASSIGNMENT((#36776));
#36770=PRESENTATION_STYLE_ASSIGNMENT((#36777));
#36771=SURFACE_STYLE_USAGE(.BOTH.,#36778);
#36772=SURFACE_STYLE_USAGE(.BOTH.,#36779);
#36773=SURFACE_STYLE_USAGE(.BOTH.,#36780);
#36774=SURFACE_STYLE_USAGE(.BOTH.,#36781);
#36775=SURFACE_STYLE_USAGE(.BOTH.,#36782);
#36776=SURFACE_STYLE_USAGE(.BOTH.,#36783);
#36777=SURFACE_STYLE_USAGE(.BOTH.,#36784);
#36778=SURFACE_SIDE_STYLE('',(#36785));
#36779=SURFACE_SIDE_STYLE('',(#36786));
#36780=SURFACE_SIDE_STYLE('',(#36787));
#36781=SURFACE_SIDE_STYLE('',(#36788));
#36782=SURFACE_SIDE_STYLE('',(#36789));
#36783=SURFACE_SIDE_STYLE('',(#36790));
#36784=SURFACE_SIDE_STYLE('',(#36791));
#36785=SURFACE_STYLE_FILL_AREA(#36792);
#36786=SURFACE_STYLE_FILL_AREA(#36793);
#36787=SURFACE_STYLE_FILL_AREA(#36794);
#36788=SURFACE_STYLE_FILL_AREA(#36795);
#36789=SURFACE_STYLE_FILL_AREA(#36796);
#36790=SURFACE_STYLE_FILL_AREA(#36797);
#36791=SURFACE_STYLE_FILL_AREA(#36798);
#36792=FILL_AREA_STYLE('Steel - Satin',(#36799));
#36793=FILL_AREA_STYLE('Opaque(23,69,131)',(#36800));
#36794=FILL_AREA_STYLE('Opaque(104,114,127)',(#36801));
#36795=FILL_AREA_STYLE('Opaque(185,192,202)',(#36802));
#36796=FILL_AREA_STYLE('Opaque(21,23,26)',(#36803));
#36797=FILL_AREA_STYLE('Opaque(81,175,227)',(#36804));
#36798=FILL_AREA_STYLE('Opaque(169,212,242)',(#36805));
#36799=FILL_AREA_STYLE_COLOUR('Steel - Satin',#36806);
#36800=FILL_AREA_STYLE_COLOUR('Opaque(23,69,131)',#36807);
#36801=FILL_AREA_STYLE_COLOUR('Opaque(104,114,127)',#36808);
#36802=FILL_AREA_STYLE_COLOUR('Opaque(185,192,202)',#36809);
#36803=FILL_AREA_STYLE_COLOUR('Opaque(21,23,26)',#36810);
#36804=FILL_AREA_STYLE_COLOUR('Opaque(81,175,227)',#36811);
#36805=FILL_AREA_STYLE_COLOUR('Opaque(169,212,242)',#36812);
#36806=COLOUR_RGB('Steel - Satin',0.627450980392157,0.627450980392157,0.627450980392157);
#36807=COLOUR_RGB('Opaque(23,69,131)',0.0901960784313725,0.270588235294118,
0.513725490196078);
#36808=COLOUR_RGB('Opaque(104,114,127)',0.407843137254902,0.447058823529412,
0.498039215686275);
#36809=COLOUR_RGB('Opaque(185,192,202)',0.725490196078431,0.752941176470588,
0.792156862745098);
#36810=COLOUR_RGB('Opaque(21,23,26)',0.0823529411764706,0.0901960784313725,
0.101960784313725);
#36811=COLOUR_RGB('Opaque(81,175,227)',0.317647058823529,0.686274509803922,
0.890196078431372);
#36812=COLOUR_RGB('Opaque(169,212,242)',0.662745098039216,0.831372549019608,
0.949019607843137);
ENDSEC;
END-ISO-10303-21;
